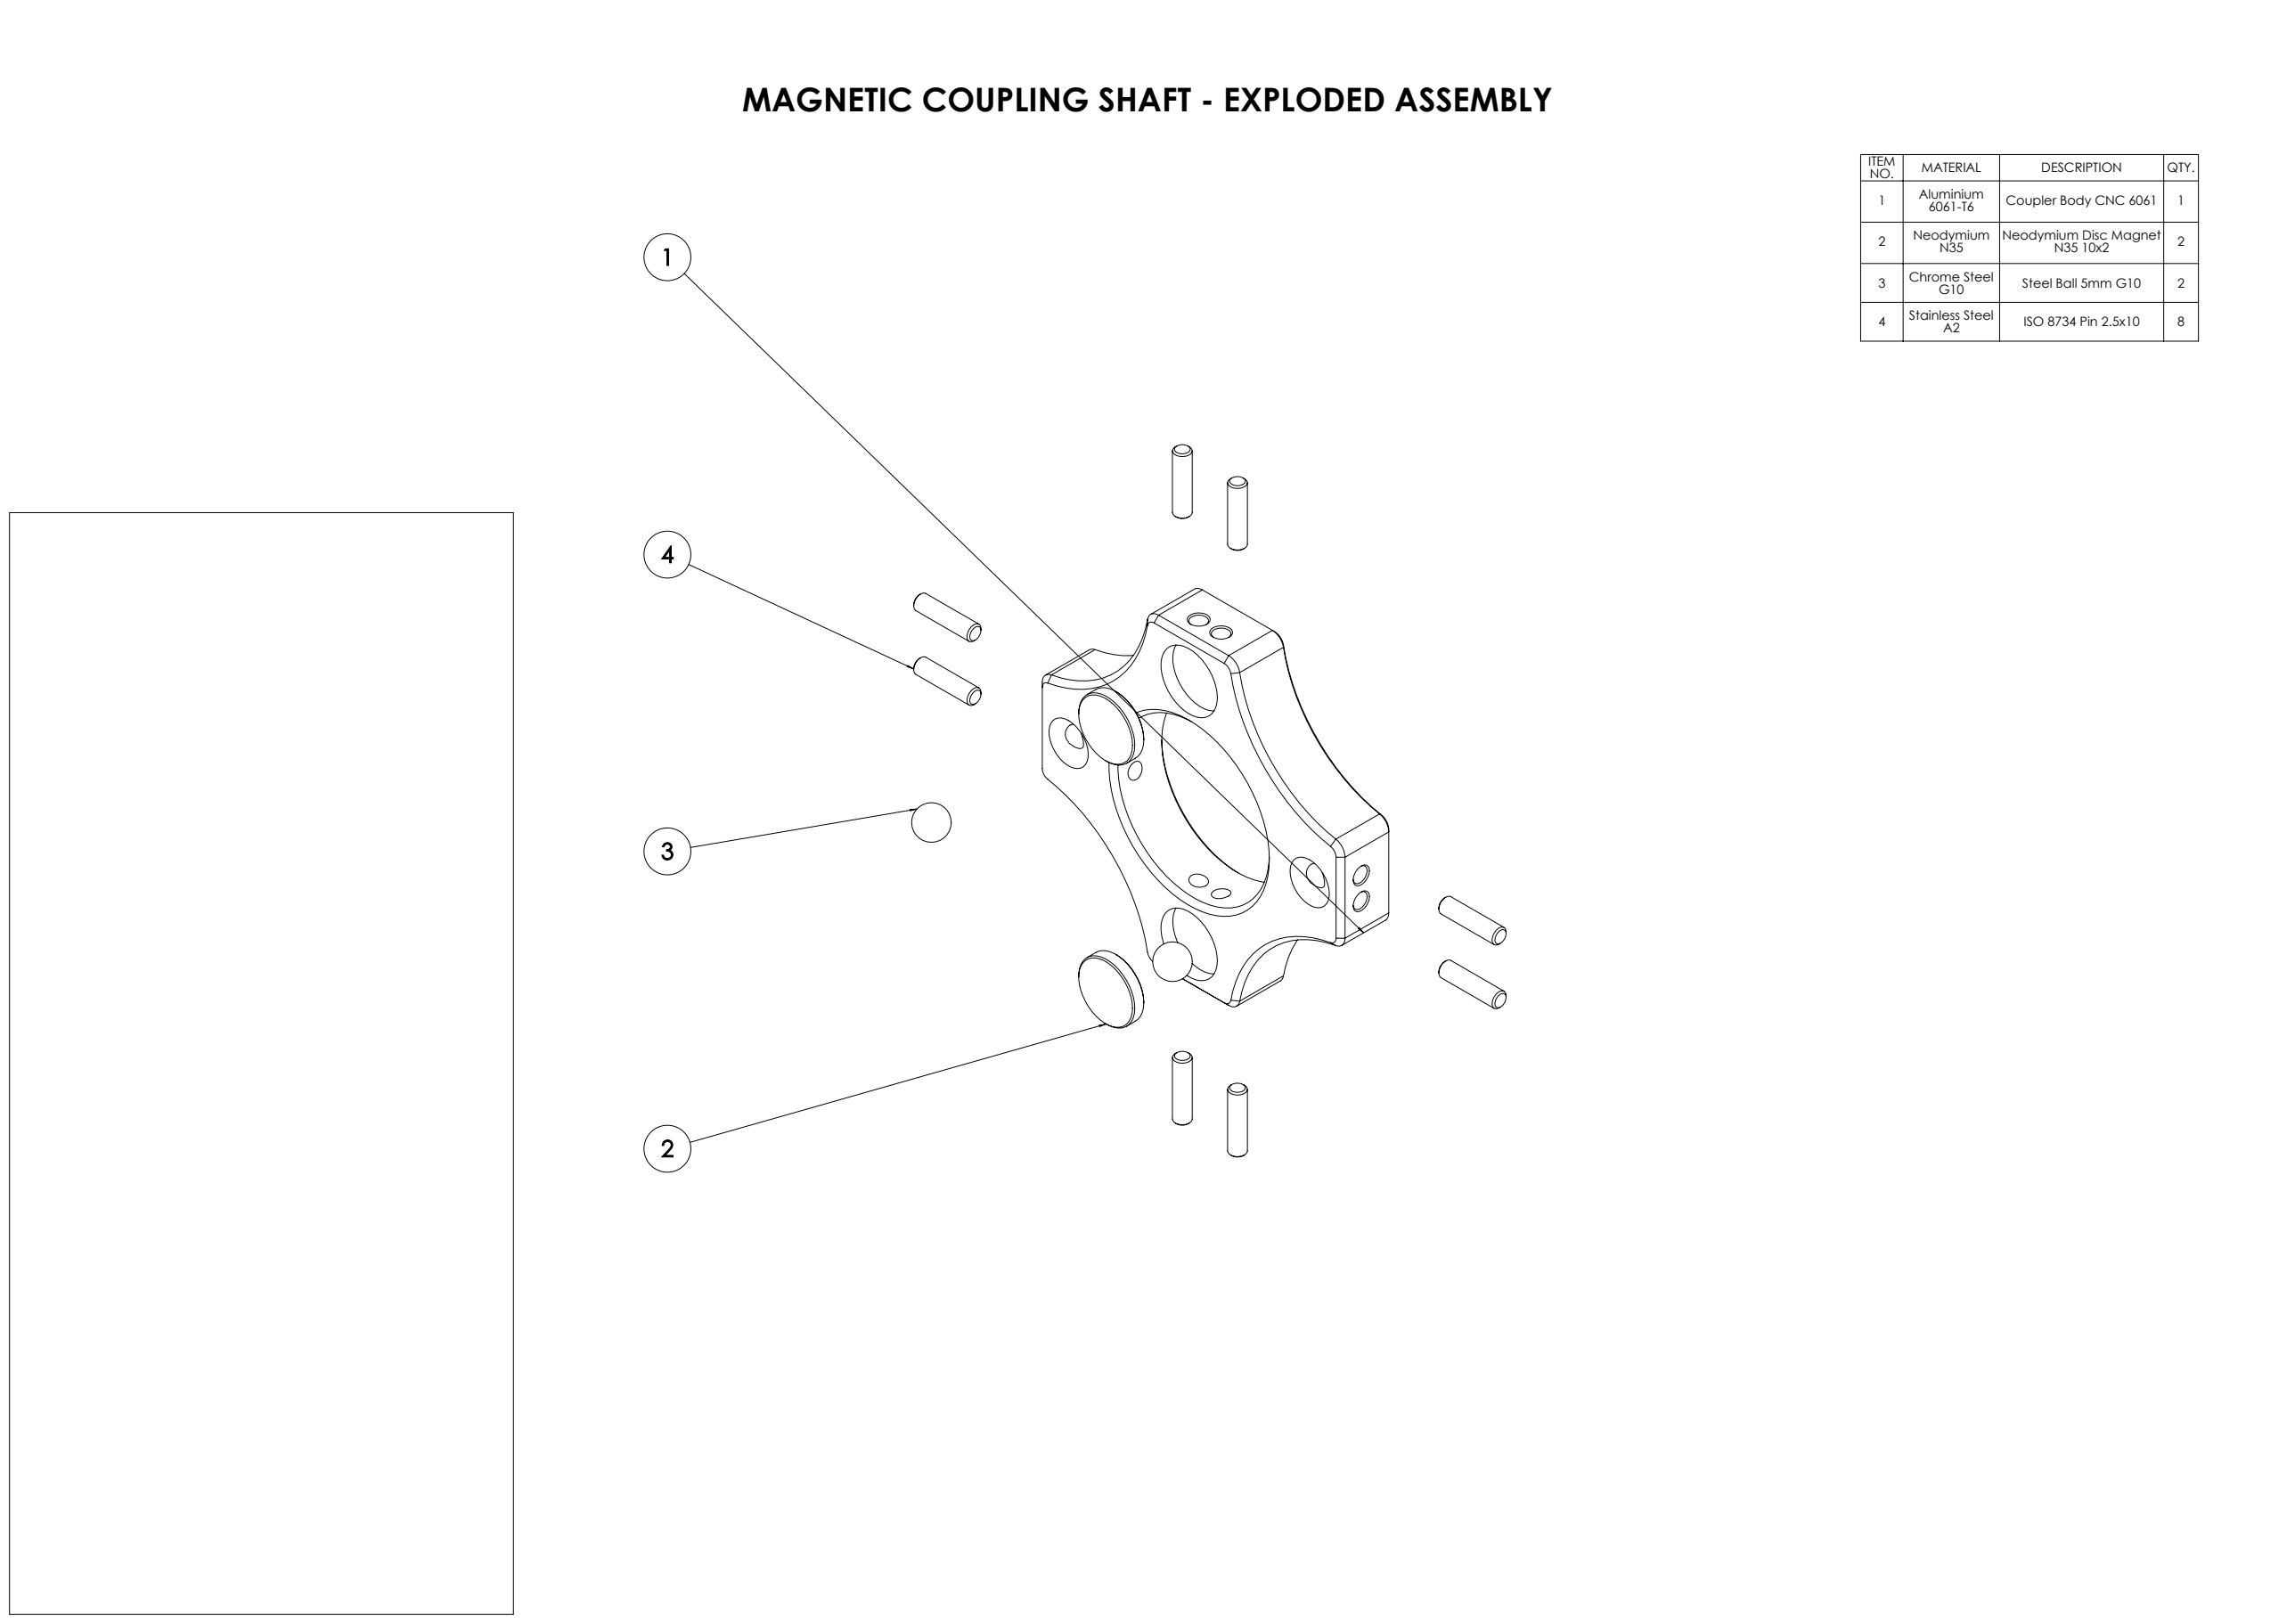
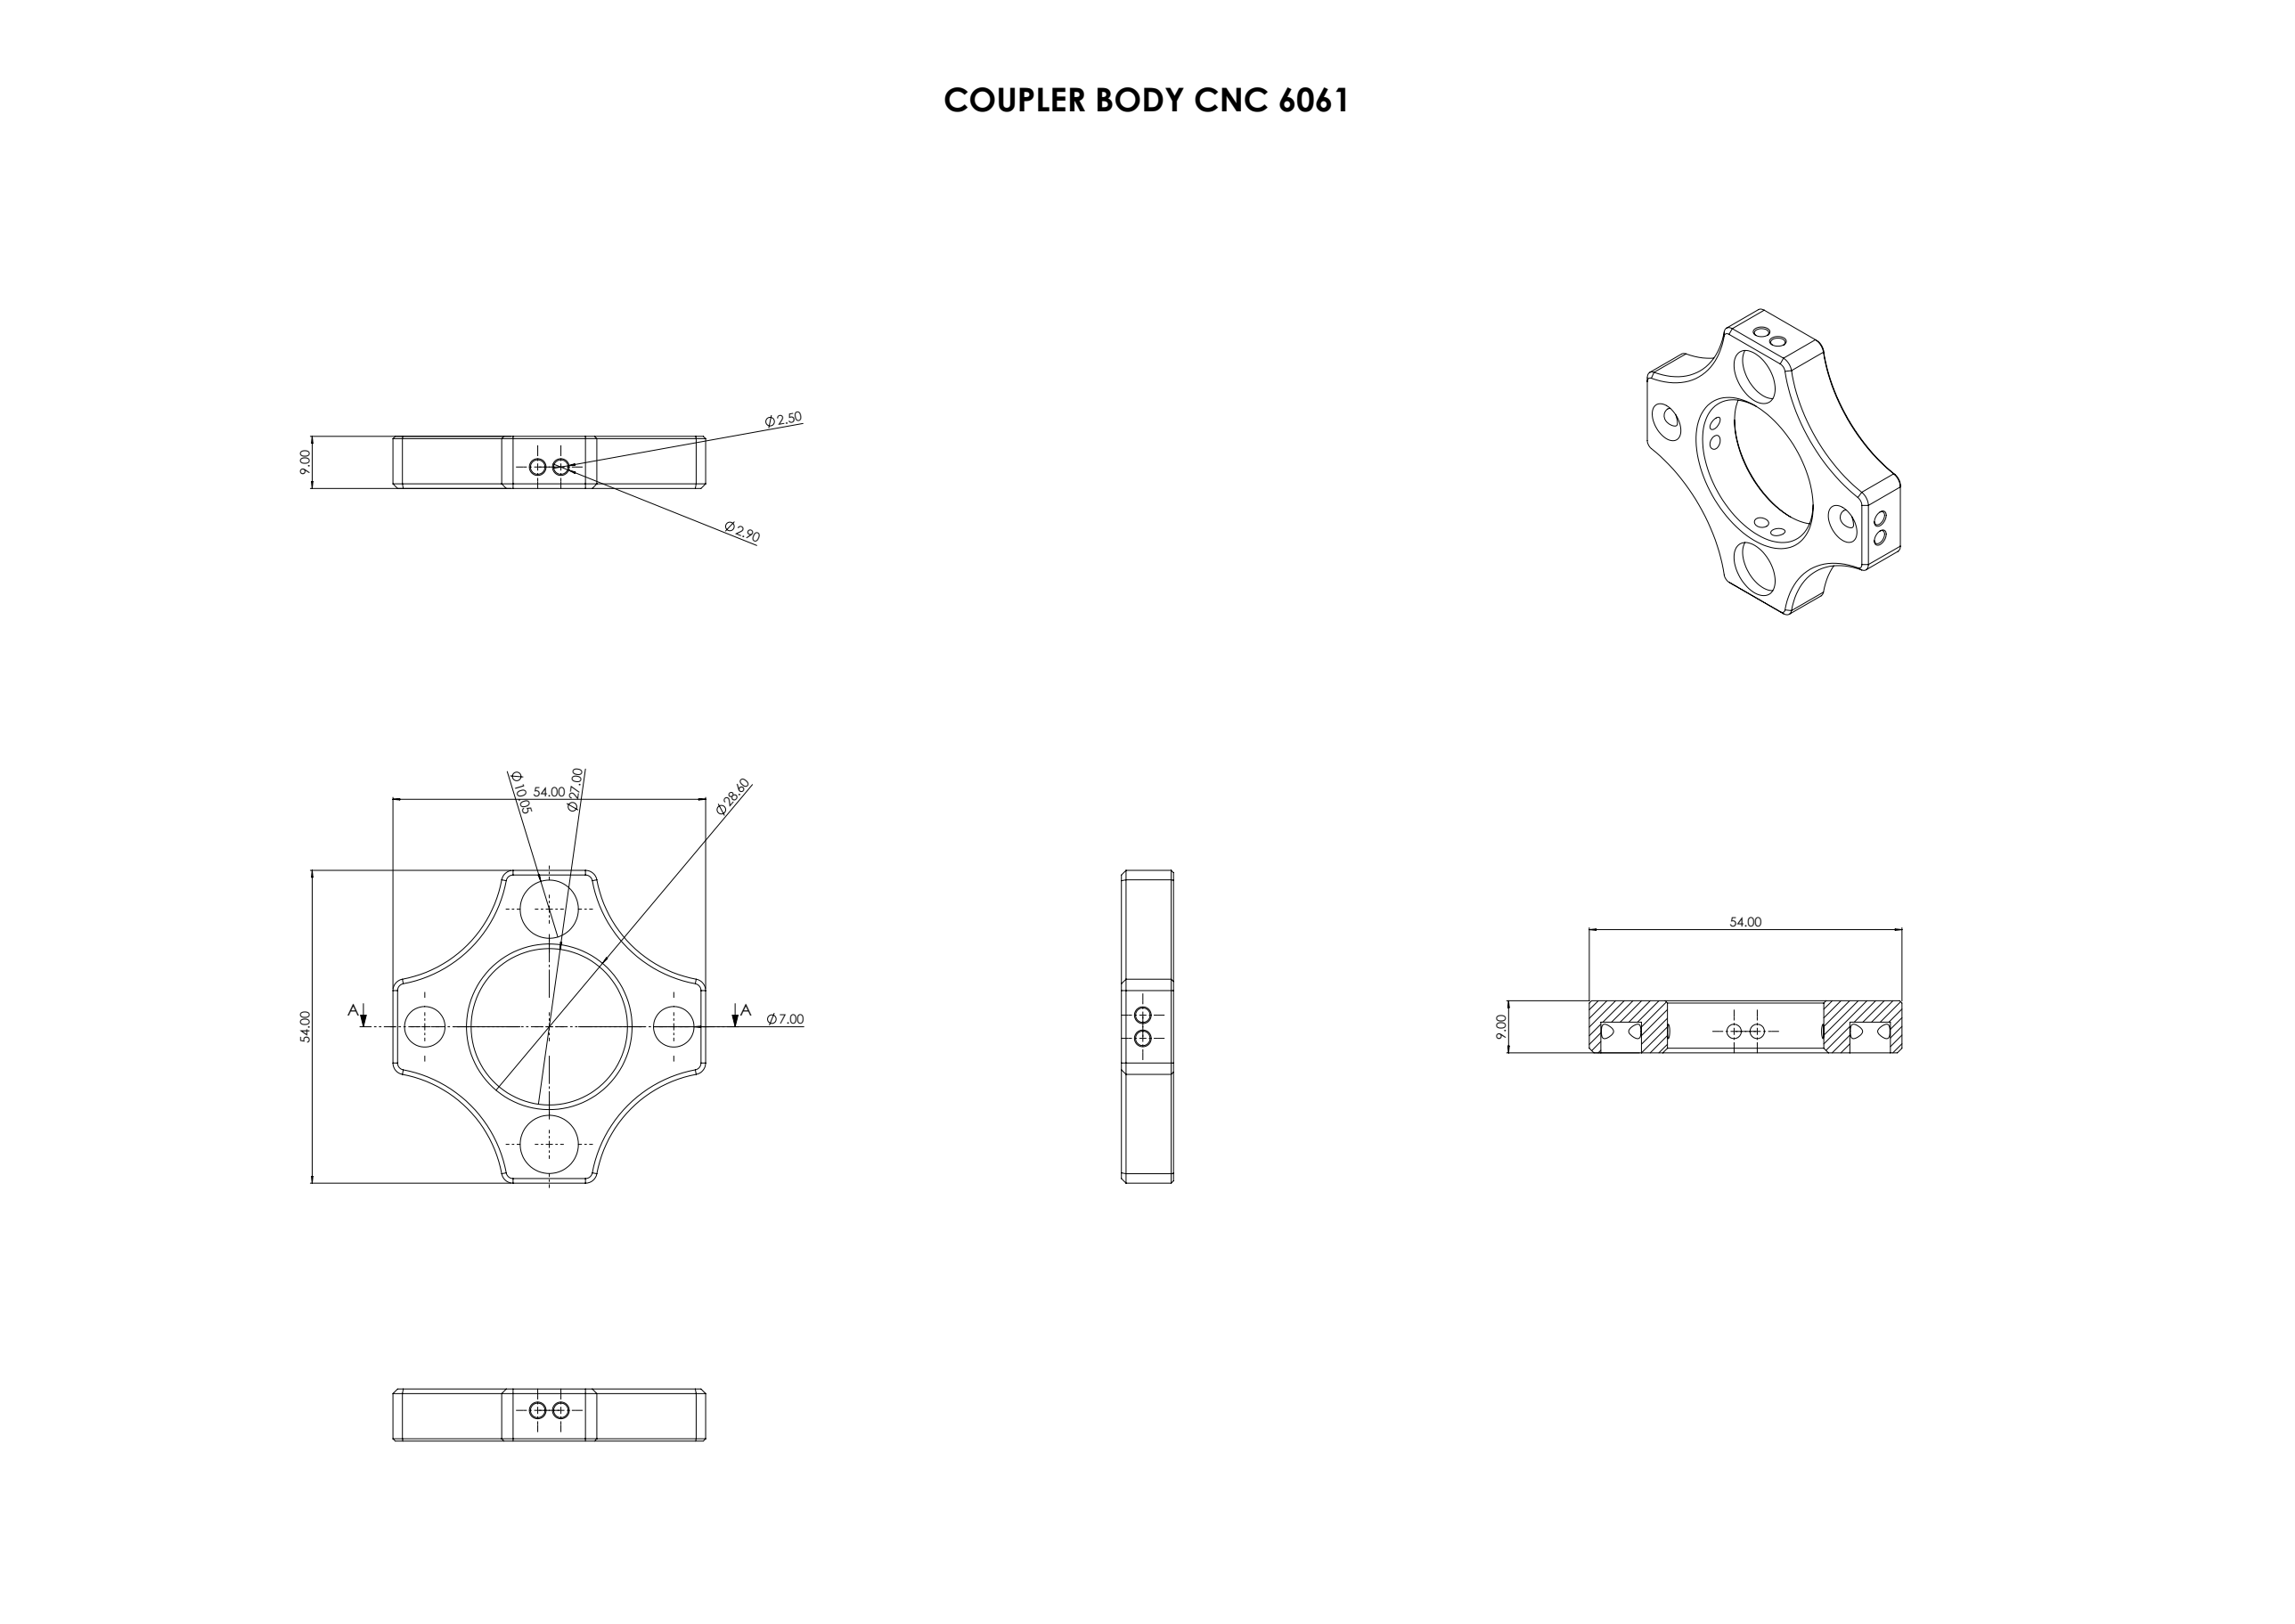
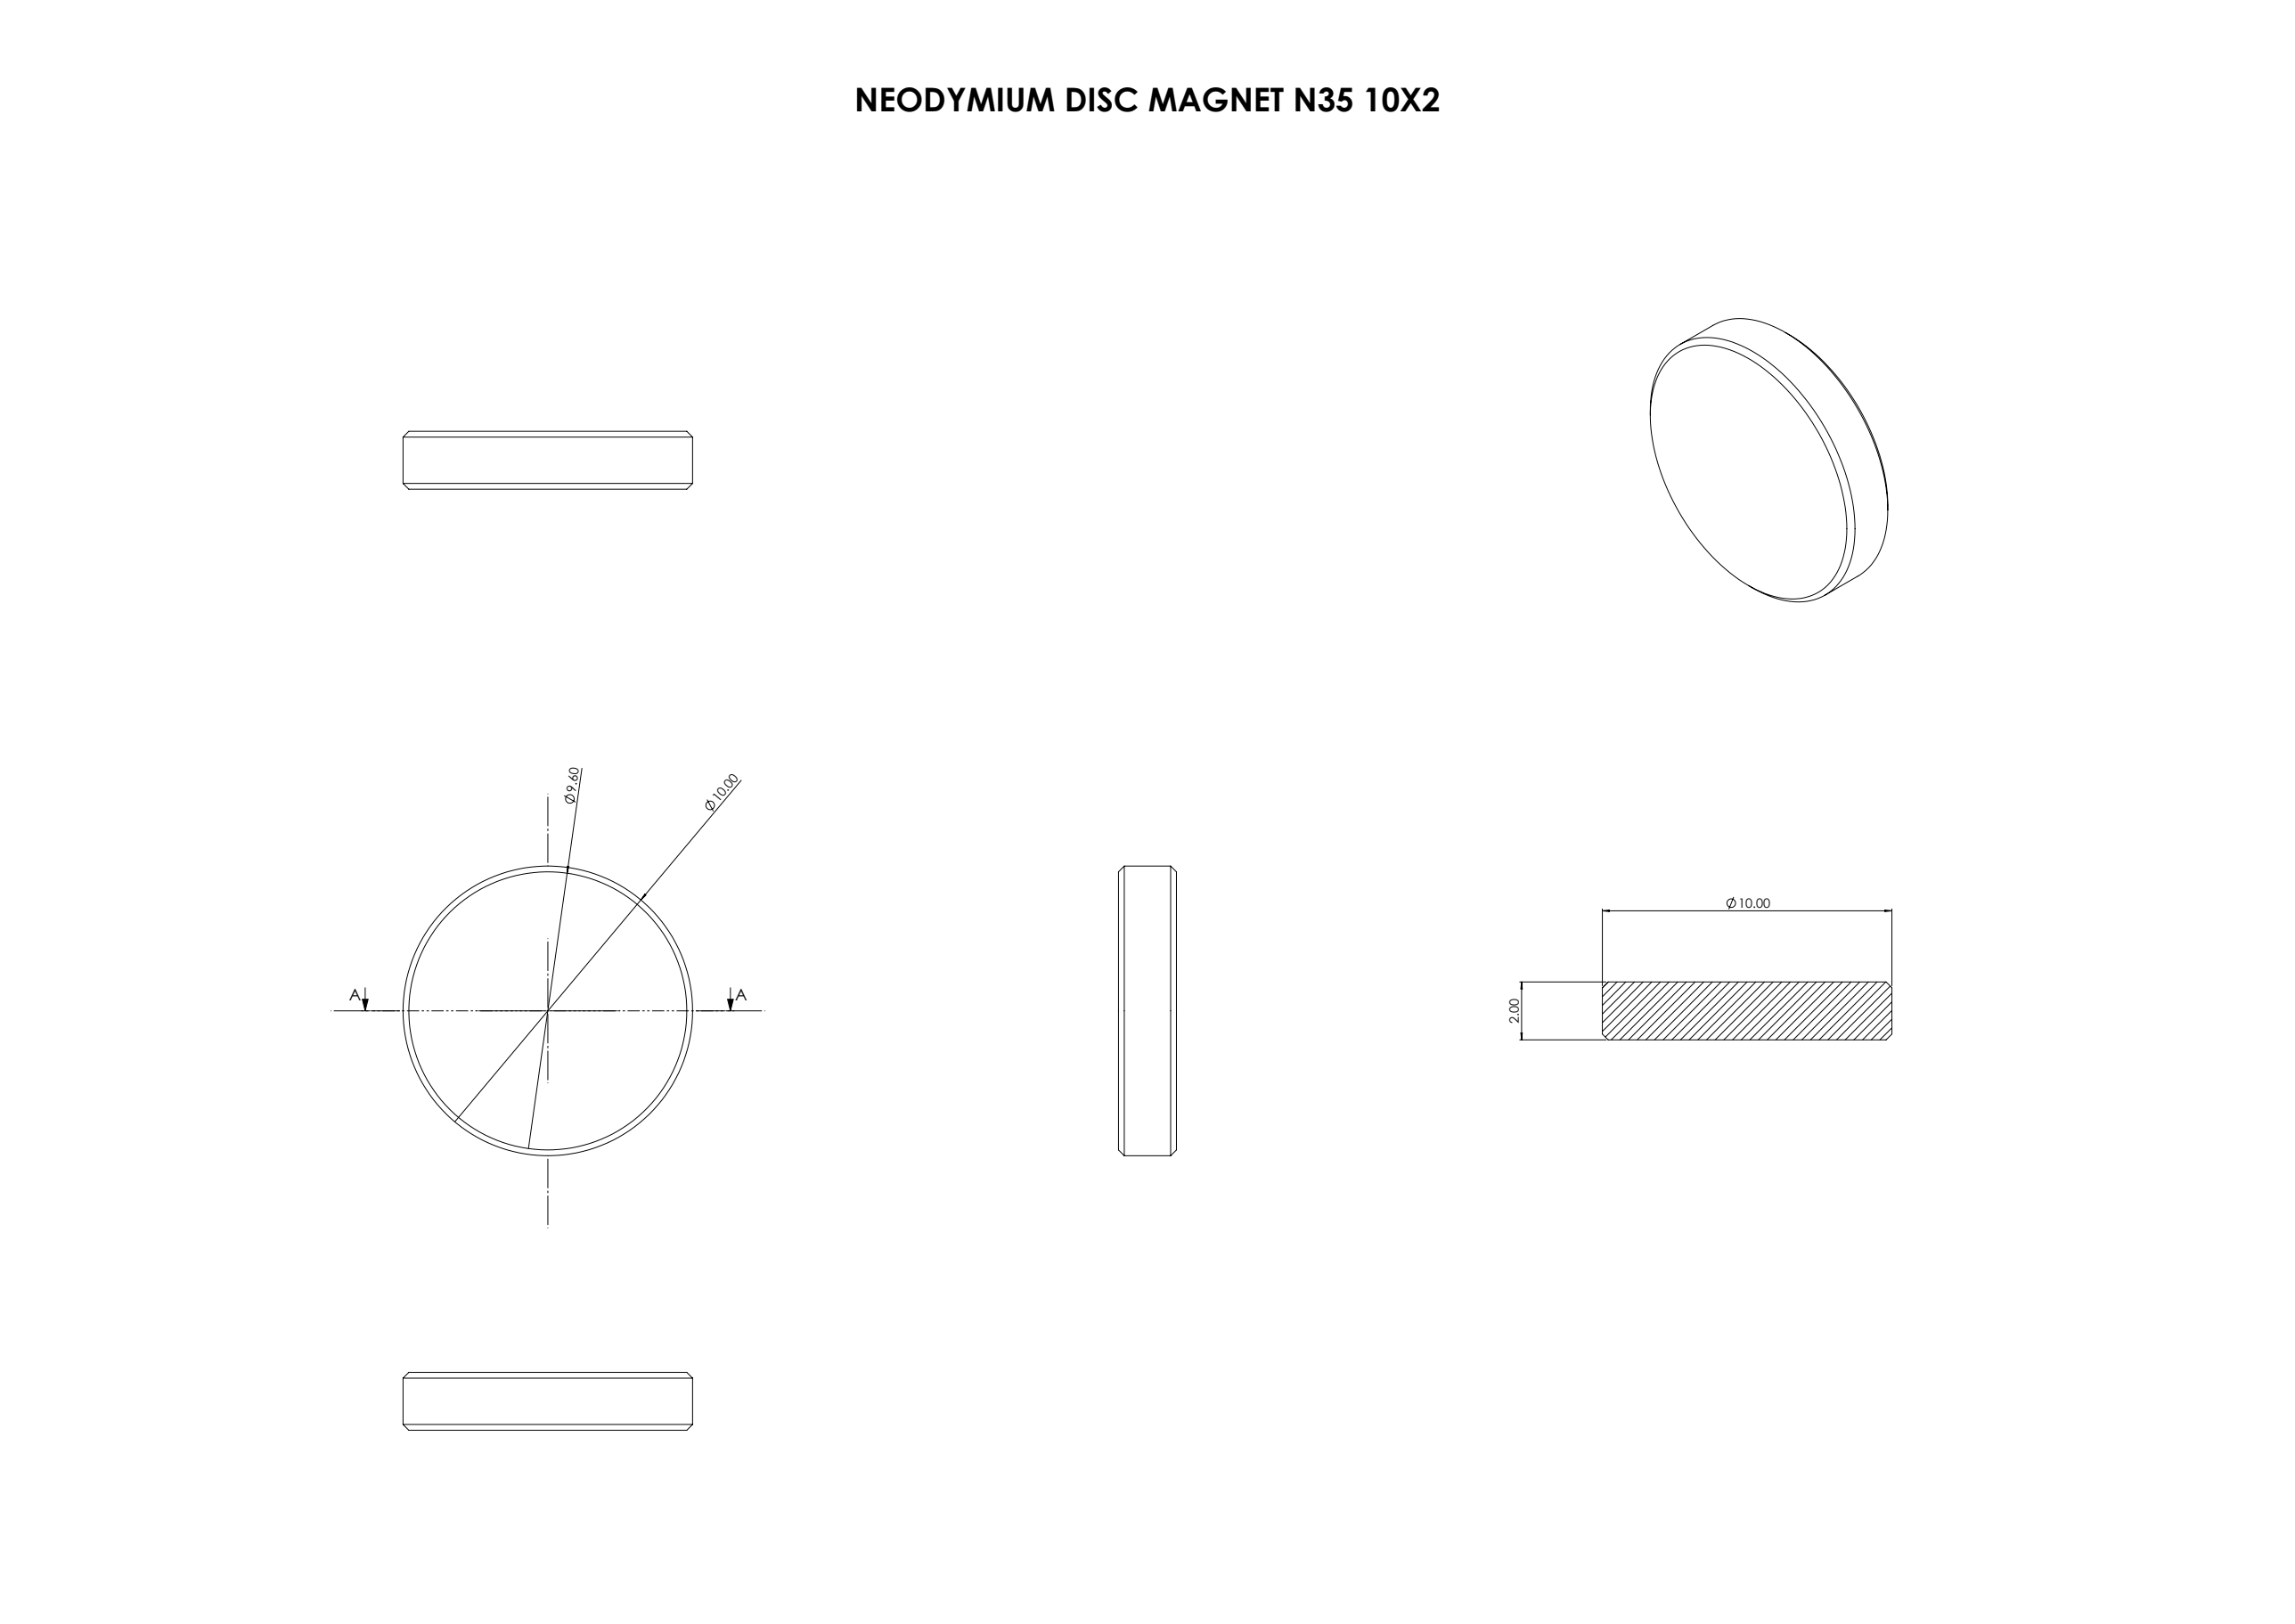
ISO-10303-21;
HEADER;
/* Generated by software containing ST-Developer
 * from STEP Tools, Inc. (www.steptools.com) 
 */

FILE_DESCRIPTION(
/* description */ (''),
/* implementation_level */ '2;1');

FILE_NAME(
/* name */ 'MAS-363',
/* time_stamp */ '2026-10-11T08:53:36-07:00',
/* author */ (''),
/* organization */ (''),
/* preprocessor_version */ 'ST-DEVELOPER v20.2',
/* originating_system */ 'Autodesk Translation Framework v15.15.0.0',
/* authorisation */ '');

FILE_SCHEMA (('AUTOMOTIVE_DESIGN { 1 0 10303 214 3 1 1 }'));
ENDSEC;

DATA;
#10=MECHANICAL_DESIGN_GEOMETRIC_PRESENTATION_REPRESENTATION('',(#72,#73,
#74,#75),#3338);
#11=ITEM_DEFINED_TRANSFORMATION($,$,#1624,#1805);
#12=ITEM_DEFINED_TRANSFORMATION($,$,#1782,#1806);
#13=ITEM_DEFINED_TRANSFORMATION($,$,#1782,#1807);
#14=ITEM_DEFINED_TRANSFORMATION($,$,#1792,#1808);
#15=ITEM_DEFINED_TRANSFORMATION($,$,#1792,#1809);
#16=ITEM_DEFINED_TRANSFORMATION($,$,#1795,#1810);
#17=ITEM_DEFINED_TRANSFORMATION($,$,#1795,#1811);
#18=ITEM_DEFINED_TRANSFORMATION($,$,#1795,#1812);
#19=ITEM_DEFINED_TRANSFORMATION($,$,#1795,#1813);
#20=ITEM_DEFINED_TRANSFORMATION($,$,#1795,#1814);
#21=ITEM_DEFINED_TRANSFORMATION($,$,#1795,#1815);
#22=ITEM_DEFINED_TRANSFORMATION($,$,#1795,#1816);
#23=ITEM_DEFINED_TRANSFORMATION($,$,#1795,#1817);
#24=(
REPRESENTATION_RELATIONSHIP($,$,#3367,#3366)
REPRESENTATION_RELATIONSHIP_WITH_TRANSFORMATION(#11)
SHAPE_REPRESENTATION_RELATIONSHIP()
);
#25=(
REPRESENTATION_RELATIONSHIP($,$,#3368,#3366)
REPRESENTATION_RELATIONSHIP_WITH_TRANSFORMATION(#12)
SHAPE_REPRESENTATION_RELATIONSHIP()
);
#26=(
REPRESENTATION_RELATIONSHIP($,$,#3368,#3366)
REPRESENTATION_RELATIONSHIP_WITH_TRANSFORMATION(#13)
SHAPE_REPRESENTATION_RELATIONSHIP()
);
#27=(
REPRESENTATION_RELATIONSHIP($,$,#3369,#3366)
REPRESENTATION_RELATIONSHIP_WITH_TRANSFORMATION(#14)
SHAPE_REPRESENTATION_RELATIONSHIP()
);
#28=(
REPRESENTATION_RELATIONSHIP($,$,#3369,#3366)
REPRESENTATION_RELATIONSHIP_WITH_TRANSFORMATION(#15)
SHAPE_REPRESENTATION_RELATIONSHIP()
);
#29=(
REPRESENTATION_RELATIONSHIP($,$,#3370,#3366)
REPRESENTATION_RELATIONSHIP_WITH_TRANSFORMATION(#16)
SHAPE_REPRESENTATION_RELATIONSHIP()
);
#30=(
REPRESENTATION_RELATIONSHIP($,$,#3370,#3366)
REPRESENTATION_RELATIONSHIP_WITH_TRANSFORMATION(#17)
SHAPE_REPRESENTATION_RELATIONSHIP()
);
#31=(
REPRESENTATION_RELATIONSHIP($,$,#3370,#3366)
REPRESENTATION_RELATIONSHIP_WITH_TRANSFORMATION(#18)
SHAPE_REPRESENTATION_RELATIONSHIP()
);
#32=(
REPRESENTATION_RELATIONSHIP($,$,#3370,#3366)
REPRESENTATION_RELATIONSHIP_WITH_TRANSFORMATION(#19)
SHAPE_REPRESENTATION_RELATIONSHIP()
);
#33=(
REPRESENTATION_RELATIONSHIP($,$,#3370,#3366)
REPRESENTATION_RELATIONSHIP_WITH_TRANSFORMATION(#20)
SHAPE_REPRESENTATION_RELATIONSHIP()
);
#34=(
REPRESENTATION_RELATIONSHIP($,$,#3370,#3366)
REPRESENTATION_RELATIONSHIP_WITH_TRANSFORMATION(#21)
SHAPE_REPRESENTATION_RELATIONSHIP()
);
#35=(
REPRESENTATION_RELATIONSHIP($,$,#3370,#3366)
REPRESENTATION_RELATIONSHIP_WITH_TRANSFORMATION(#22)
SHAPE_REPRESENTATION_RELATIONSHIP()
);
#36=(
REPRESENTATION_RELATIONSHIP($,$,#3370,#3366)
REPRESENTATION_RELATIONSHIP_WITH_TRANSFORMATION(#23)
SHAPE_REPRESENTATION_RELATIONSHIP()
);
#37=CONTEXT_DEPENDENT_SHAPE_REPRESENTATION(#24,#3353);
#38=CONTEXT_DEPENDENT_SHAPE_REPRESENTATION(#25,#3354);
#39=CONTEXT_DEPENDENT_SHAPE_REPRESENTATION(#26,#3355);
#40=CONTEXT_DEPENDENT_SHAPE_REPRESENTATION(#27,#3356);
#41=CONTEXT_DEPENDENT_SHAPE_REPRESENTATION(#28,#3357);
#42=CONTEXT_DEPENDENT_SHAPE_REPRESENTATION(#29,#3358);
#43=CONTEXT_DEPENDENT_SHAPE_REPRESENTATION(#30,#3359);
#44=CONTEXT_DEPENDENT_SHAPE_REPRESENTATION(#31,#3360);
#45=CONTEXT_DEPENDENT_SHAPE_REPRESENTATION(#32,#3361);
#46=CONTEXT_DEPENDENT_SHAPE_REPRESENTATION(#33,#3362);
#47=CONTEXT_DEPENDENT_SHAPE_REPRESENTATION(#34,#3363);
#48=CONTEXT_DEPENDENT_SHAPE_REPRESENTATION(#35,#3364);
#49=CONTEXT_DEPENDENT_SHAPE_REPRESENTATION(#36,#3365);
#50=NEXT_ASSEMBLY_USAGE_OCCURRENCE('01_Coupler_Body_CNC_6061:2',
'01_Coupler_Body_CNC_6061:2','01_Coupler_Body_CNC_6061:2',#3372,#3373,
'01_Coupler_Body_CNC_6061:2');
#51=NEXT_ASSEMBLY_USAGE_OCCURRENCE(
'02_Neodymium_Disc_Magnet_N35_10x2:2',
'02_Neodymium_Disc_Magnet_N35_10x2:2',
'02_Neodymium_Disc_Magnet_N35_10x2:2',#3372,#3374,
'02_Neodymium_Disc_Magnet_N35_10x2:2');
#52=NEXT_ASSEMBLY_USAGE_OCCURRENCE(
'02_Neodymium_Disc_Magnet_N35_10x2:3',
'02_Neodymium_Disc_Magnet_N35_10x2:3',
'02_Neodymium_Disc_Magnet_N35_10x2:3',#3372,#3374,
'02_Neodymium_Disc_Magnet_N35_10x2:3');
#53=NEXT_ASSEMBLY_USAGE_OCCURRENCE('03_Steel_Ball_5mm_G10:2',
'03_Steel_Ball_5mm_G10:2','03_Steel_Ball_5mm_G10:2',#3372,#3375,
'03_Steel_Ball_5mm_G10:2');
#54=NEXT_ASSEMBLY_USAGE_OCCURRENCE('03_Steel_Ball_5mm_G10:3',
'03_Steel_Ball_5mm_G10:3','03_Steel_Ball_5mm_G10:3',#3372,#3375,
'03_Steel_Ball_5mm_G10:3');
#55=NEXT_ASSEMBLY_USAGE_OCCURRENCE('04_ISO_8734_Pin_2.5x10:2',
'04_ISO_8734_Pin_2.5x10:2','04_ISO_8734_Pin_2.5x10:2',#3372,#3376,
'04_ISO_8734_Pin_2.5x10:2');
#56=NEXT_ASSEMBLY_USAGE_OCCURRENCE('04_ISO_8734_Pin_2.5x10:3',
'04_ISO_8734_Pin_2.5x10:3','04_ISO_8734_Pin_2.5x10:3',#3372,#3376,
'04_ISO_8734_Pin_2.5x10:3');
#57=NEXT_ASSEMBLY_USAGE_OCCURRENCE('04_ISO_8734_Pin_2.5x10:4',
'04_ISO_8734_Pin_2.5x10:4','04_ISO_8734_Pin_2.5x10:4',#3372,#3376,
'04_ISO_8734_Pin_2.5x10:4');
#58=NEXT_ASSEMBLY_USAGE_OCCURRENCE('04_ISO_8734_Pin_2.5x10:5',
'04_ISO_8734_Pin_2.5x10:5','04_ISO_8734_Pin_2.5x10:5',#3372,#3376,
'04_ISO_8734_Pin_2.5x10:5');
#59=NEXT_ASSEMBLY_USAGE_OCCURRENCE('04_ISO_8734_Pin_2.5x10:6',
'04_ISO_8734_Pin_2.5x10:6','04_ISO_8734_Pin_2.5x10:6',#3372,#3376,
'04_ISO_8734_Pin_2.5x10:6');
#60=NEXT_ASSEMBLY_USAGE_OCCURRENCE('04_ISO_8734_Pin_2.5x10:7',
'04_ISO_8734_Pin_2.5x10:7','04_ISO_8734_Pin_2.5x10:7',#3372,#3376,
'04_ISO_8734_Pin_2.5x10:7');
#61=NEXT_ASSEMBLY_USAGE_OCCURRENCE('04_ISO_8734_Pin_2.5x10:8',
'04_ISO_8734_Pin_2.5x10:8','04_ISO_8734_Pin_2.5x10:8',#3372,#3376,
'04_ISO_8734_Pin_2.5x10:8');
#62=NEXT_ASSEMBLY_USAGE_OCCURRENCE('04_ISO_8734_Pin_2.5x10:9',
'04_ISO_8734_Pin_2.5x10:9','04_ISO_8734_Pin_2.5x10:9',#3372,#3376,
'04_ISO_8734_Pin_2.5x10:9');
#63=SPHERICAL_SURFACE('',#1793,2.5);
#64=SHAPE_REPRESENTATION_RELATIONSHIP('SRR','None',#3367,#68);
#65=SHAPE_REPRESENTATION_RELATIONSHIP('SRR','None',#3368,#69);
#66=SHAPE_REPRESENTATION_RELATIONSHIP('SRR','None',#3369,#70);
#67=SHAPE_REPRESENTATION_RELATIONSHIP('SRR','None',#3370,#71);
#68=ADVANCED_BREP_SHAPE_REPRESENTATION('',(#76),#3334);
#69=ADVANCED_BREP_SHAPE_REPRESENTATION('',(#77),#3335);
#70=ADVANCED_BREP_SHAPE_REPRESENTATION('',(#78),#3336);
#71=ADVANCED_BREP_SHAPE_REPRESENTATION('',(#79),#3337);
#72=STYLED_ITEM('',(#3436),#76);
#73=STYLED_ITEM('',(#3450),#77);
#74=STYLED_ITEM('',(#3443),#78);
#75=STYLED_ITEM('',(#3457),#79);
#76=MANIFOLD_SOLID_BREP('Body1',#1574);
#77=MANIFOLD_SOLID_BREP('Body1',#1575);
#78=MANIFOLD_SOLID_BREP('Body1',#1576);
#79=MANIFOLD_SOLID_BREP('Body1',#1577);
#80=B_SPLINE_CURVE_WITH_KNOTS('',3,(#2327,#2328,#2329,#2330,#2331,#2332,
#2333,#2334,#2335,#2336),.UNSPECIFIED.,.F.,.F.,(4,2,2,2,4),(0.,0.0466731196164697,
0.0933462392329394,0.146281754847064,0.199217270461189),.UNSPECIFIED.);
#81=B_SPLINE_CURVE_WITH_KNOTS('',3,(#2337,#2338,#2339,#2340,#2341,#2342,
#2343,#2344,#2345,#2346,#2347,#2348,#2349,#2350,#2351,#2352,#2353,#2354,
#2355,#2356,#2357,#2358,#2359,#2360,#2361,#2362,#2363,#2364,#2365,#2366),
 .UNSPECIFIED.,.F.,.F.,(4,2,2,2,2,2,2,2,2,2,2,2,2,2,4),(0.199217270461189,
0.269430202694905,0.339643134928622,0.393818540201201,0.42090624283749,
0.44799394547378,0.475081648110069,0.502169350746359,0.556344756018938,
0.626557688252654,0.696770620486371,0.749706136100495,0.80264165171462,
0.84931477133109,0.895987890947559),.UNSPECIFIED.);
#82=B_SPLINE_CURVE_WITH_KNOTS('',3,(#2389,#2390,#2391,#2392,#2393,#2394,
#2395,#2396,#2397,#2398,#2399,#2400,#2401,#2402,#2403,#2404,#2405,#2406,
#2407,#2408,#2409,#2410,#2411,#2412,#2413,#2414,#2415,#2416,#2417,#2418),
 .UNSPECIFIED.,.F.,.F.,(4,2,2,2,2,2,2,2,2,2,2,2,2,2,4),(0.,0.0466731196164697,
0.0933462392329393,0.146281754847064,0.199217270461189,0.269430202694905,
0.339643134928622,0.393818540201201,0.42090624283749,0.44799394547378,0.475081648110069,
0.502169350746358,0.556344756018937,0.626557688252654,0.69677062048637),
 .UNSPECIFIED.);
#83=B_SPLINE_CURVE_WITH_KNOTS('',3,(#2419,#2420,#2421,#2422,#2423,#2424,
#2425,#2426,#2427,#2428),.UNSPECIFIED.,.F.,.F.,(4,2,2,2,4),(0.69677062048637,
0.749706136100495,0.80264165171462,0.84931477133109,0.895987890947559),
 .UNSPECIFIED.);
#84=B_SPLINE_CURVE_WITH_KNOTS('',3,(#2436,#2437,#2438,#2439,#2440,#2441,
#2442,#2443,#2444,#2445,#2446,#2447),.UNSPECIFIED.,.F.,.F.,(4,2,2,2,2,4),
(0.,0.0270877026362895,0.054175405272579,0.108350810545158,0.178563742778874,
0.248776675012591),.UNSPECIFIED.);
#85=B_SPLINE_CURVE_WITH_KNOTS('',3,(#2448,#2449,#2450,#2451,#2452,#2453,
#2454,#2455,#2456,#2457,#2458,#2459,#2460,#2461,#2462,#2463,#2464,#2465,
#2466,#2467,#2468,#2469,#2470,#2471,#2472,#2473,#2474,#2475),
 .UNSPECIFIED.,.F.,.F.,(4,2,2,2,2,2,2,2,2,2,2,2,2,4),(0.248776675012591,
0.301712190626716,0.35464770624084,0.40132082585731,0.44799394547378,0.494667065090249,
0.541340184706719,0.594275700320844,0.647211215934968,0.717424148168685,
0.787637080402401,0.84181248567498,0.86890018831127,0.895987890947559),
 .UNSPECIFIED.);
#86=B_SPLINE_CURVE_WITH_KNOTS('',3,(#2485,#2486,#2487,#2488,#2489,#2490,
#2491,#2492,#2493,#2494,#2495,#2496,#2497,#2498,#2499,#2500,#2501,#2502,
#2503,#2504,#2505,#2506,#2507,#2508,#2509,#2510,#2511,#2512),
 .UNSPECIFIED.,.F.,.F.,(4,2,2,2,2,2,2,2,2,2,2,2,2,4),(0.,0.0270877026362894,
0.0541754052725788,0.108350810545158,0.178563742778874,0.248776675012591,
0.301712190626716,0.35464770624084,0.40132082585731,0.44799394547378,0.494667065090249,
0.541340184706719,0.594275700320844,0.647211215934968),.UNSPECIFIED.);
#87=B_SPLINE_CURVE_WITH_KNOTS('',3,(#2513,#2514,#2515,#2516,#2517,#2518,
#2519,#2520,#2521,#2522,#2523,#2524),.UNSPECIFIED.,.F.,.F.,(4,2,2,2,2,4),
(0.647211215934968,0.717424148168685,0.787637080402402,0.84181248567498,
0.86890018831127,0.895987890947559),.UNSPECIFIED.);
#88=B_SPLINE_CURVE_WITH_KNOTS('',3,(#2544,#2545,#2546,#2547,#2548,#2549,
#2550,#2551,#2552,#2553,#2554,#2555,#2556,#2557,#2558,#2559,#2560,#2561,
#2562,#2563,#2564,#2565,#2566,#2567,#2568,#2569,#2570,#2571,#2572,#2573,
#2574,#2575,#2576,#2577),.UNSPECIFIED.,.T.,.F.,(4,2,2,2,2,2,2,2,2,2,2,2,
2,2,2,2,4),(0.,0.0471177022580085,0.094235404516017,0.142168460352567,0.190101516189116,
0.237513099195747,0.284924682202378,0.331987109916568,0.379049537630759,
0.426111965344949,0.473174393059139,0.52058597606577,0.567997559072401,
0.615930614908951,0.6638636707455,0.710981373003508,0.758099075261517),
 .UNSPECIFIED.);
#89=B_SPLINE_CURVE_WITH_KNOTS('',3,(#2599,#2600,#2601,#2602,#2603,#2604,
#2605,#2606,#2607,#2608,#2609,#2610,#2611,#2612,#2613,#2614,#2615,#2616,
#2617,#2618,#2619,#2620,#2621,#2622,#2623,#2624,#2625,#2626,#2627,#2628,
#2629,#2630,#2631,#2632),.UNSPECIFIED.,.T.,.F.,(4,2,2,2,2,2,2,2,2,2,2,2,
2,2,2,2,4),(0.,0.0471177022580085,0.094235404516017,0.142168460352567,0.190101516189116,
0.237513099195747,0.284924682202378,0.331987109916568,0.379049537630758,
0.426111965344949,0.473174393059139,0.52058597606577,0.567997559072401,
0.615930614908951,0.6638636707455,0.710981373003509,0.758099075261517),
 .UNSPECIFIED.);
#90=B_SPLINE_CURVE_WITH_KNOTS('',3,(#2639,#2640,#2641,#2642,#2643,#2644,
#2645,#2646,#2647,#2648,#2649,#2650,#2651,#2652,#2653,#2654,#2655,#2656,
#2657,#2658,#2659,#2660,#2661,#2662,#2663,#2664,#2665,#2666,#2667,#2668,
#2669,#2670,#2671,#2672),.UNSPECIFIED.,.T.,.F.,(4,2,2,2,2,2,2,2,2,2,2,2,
2,2,2,2,4),(0.,0.0470624277141901,0.0941248554283803,0.141536438435011,
0.188948021441642,0.236881077278192,0.284814133114742,0.33193183537275,
0.379049537630759,0.426167239888767,0.473284942146776,0.521217997983325,
0.569151053819875,0.616562636826506,0.663974219833137,0.711036647547327,
0.758099075261517),.UNSPECIFIED.);
#91=B_SPLINE_CURVE_WITH_KNOTS('',3,(#2681,#2682,#2683,#2684,#2685,#2686,
#2687,#2688,#2689,#2690,#2691,#2692,#2693,#2694,#2695,#2696,#2697,#2698,
#2699,#2700,#2701,#2702,#2703,#2704,#2705,#2706,#2707,#2708,#2709,#2710,
#2711,#2712,#2713,#2714),.UNSPECIFIED.,.T.,.F.,(4,2,2,2,2,2,2,2,2,2,2,2,
2,2,2,2,4),(0.,0.0470624277141901,0.0941248554283803,0.141536438435011,
0.188948021441642,0.236881077278192,0.284814133114742,0.33193183537275,
0.379049537630759,0.426167239888767,0.473284942146776,0.521217997983325,
0.569151053819875,0.616562636826506,0.663974219833137,0.711036647547327,
0.758099075261517),.UNSPECIFIED.);
#92=B_SPLINE_CURVE_WITH_KNOTS('',3,(#2718,#2719,#2720,#2721,#2722,#2723,
#2724,#2725,#2726,#2727,#2728,#2729),.UNSPECIFIED.,.F.,.F.,(4,2,2,2,2,4),
(0.,0.0270877026362894,0.0541754052725789,0.108350810545158,0.178563742778874,
0.248776675012591),.UNSPECIFIED.);
#93=B_SPLINE_CURVE_WITH_KNOTS('',3,(#2730,#2731,#2732,#2733,#2734,#2735,
#2736,#2737,#2738,#2739,#2740,#2741,#2742,#2743,#2744,#2745,#2746,#2747,
#2748,#2749,#2750,#2751,#2752,#2753,#2754,#2755,#2756,#2757),
 .UNSPECIFIED.,.F.,.F.,(4,2,2,2,2,2,2,2,2,2,2,2,2,4),(0.248776675012591,
0.301712190626716,0.35464770624084,0.40132082585731,0.44799394547378,0.494667065090249,
0.541340184706719,0.594275700320844,0.647211215934968,0.717424148168685,
0.787637080402401,0.84181248567498,0.86890018831127,0.895987890947559),
 .UNSPECIFIED.);
#94=B_SPLINE_CURVE_WITH_KNOTS('',3,(#2761,#2762,#2763,#2764,#2765,#2766,
#2767,#2768,#2769,#2770,#2771,#2772,#2773,#2774,#2775,#2776,#2777,#2778,
#2779,#2780,#2781,#2782,#2783,#2784,#2785,#2786),.UNSPECIFIED.,.F.,.F.,
(4,2,2,2,2,2,2,2,2,2,2,2,4),(0.,0.0471177022580085,0.094235404516017,0.142168460352567,
0.190101516189116,0.237513099195747,0.284924682202378,0.331987109916568,
0.379049537630759,0.426111965344949,0.473174393059139,0.52058597606577,
0.567997559072401),.UNSPECIFIED.);
#95=B_SPLINE_CURVE_WITH_KNOTS('',3,(#2787,#2788,#2789,#2790,#2791,#2792,
#2793,#2794,#2795,#2796),.UNSPECIFIED.,.F.,.F.,(4,2,2,2,4),(0.567997559072401,
0.615930614908951,0.6638636707455,0.710981373003509,0.758099075261517),
 .UNSPECIFIED.);
#96=B_SPLINE_CURVE_WITH_KNOTS('',3,(#2800,#2801,#2802,#2803,#2804,#2805,
#2806,#2807,#2808,#2809),.UNSPECIFIED.,.F.,.F.,(4,2,2,2,4),(0.,0.0471177022580085,
0.094235404516017,0.142168460352567,0.190101516189116),.UNSPECIFIED.);
#97=B_SPLINE_CURVE_WITH_KNOTS('',3,(#2810,#2811,#2812,#2813,#2814,#2815,
#2816,#2817,#2818,#2819,#2820,#2821,#2822,#2823,#2824,#2825,#2826,#2827,
#2828,#2829,#2830,#2831,#2832,#2833,#2834,#2835),.UNSPECIFIED.,.F.,.F.,
(4,2,2,2,2,2,2,2,2,2,2,2,4),(0.190101516189116,0.237513099195747,0.284924682202378,
0.331987109916568,0.379049537630759,0.426111965344949,0.473174393059139,
0.52058597606577,0.567997559072401,0.615930614908951,0.6638636707455,0.710981373003509,
0.758099075261517),.UNSPECIFIED.);
#98=B_SPLINE_CURVE_WITH_KNOTS('',3,(#2839,#2840,#2841,#2842,#2843,#2844,
#2845,#2846,#2847,#2848,#2849,#2850,#2851,#2852,#2853,#2854,#2855,#2856,
#2857,#2858,#2859,#2860,#2861,#2862,#2863,#2864,#2865,#2866),
 .UNSPECIFIED.,.F.,.F.,(4,2,2,2,2,2,2,2,2,2,2,2,2,4),(0.,0.0270877026362895,
0.0541754052725789,0.108350810545158,0.178563742778874,0.248776675012591,
0.301712190626716,0.35464770624084,0.40132082585731,0.44799394547378,0.494667065090249,
0.541340184706719,0.594275700320844,0.647211215934968),.UNSPECIFIED.);
#99=B_SPLINE_CURVE_WITH_KNOTS('',3,(#2867,#2868,#2869,#2870,#2871,#2872,
#2873,#2874,#2875,#2876,#2877,#2878),.UNSPECIFIED.,.F.,.F.,(4,2,2,2,2,4),
(0.647211215934968,0.717424148168685,0.787637080402401,0.84181248567498,
0.86890018831127,0.895987890947559),.UNSPECIFIED.);
#100=B_SPLINE_CURVE_WITH_KNOTS('',3,(#2882,#2883,#2884,#2885,#2886,#2887,
#2888,#2889,#2890,#2891),.UNSPECIFIED.,.F.,.F.,(4,2,2,2,4),(0.,0.0466731196164697,
0.0933462392329394,0.146281754847064,0.199217270461189),.UNSPECIFIED.);
#101=B_SPLINE_CURVE_WITH_KNOTS('',3,(#2892,#2893,#2894,#2895,#2896,#2897,
#2898,#2899,#2900,#2901,#2902,#2903,#2904,#2905,#2906,#2907,#2908,#2909,
#2910,#2911,#2912,#2913,#2914,#2915,#2916,#2917,#2918,#2919,#2920,#2921),
 .UNSPECIFIED.,.F.,.F.,(4,2,2,2,2,2,2,2,2,2,2,2,2,2,4),(0.199217270461189,
0.269430202694905,0.339643134928622,0.393818540201201,0.42090624283749,
0.44799394547378,0.475081648110069,0.502169350746359,0.556344756018938,
0.626557688252654,0.696770620486371,0.749706136100496,0.80264165171462,
0.84931477133109,0.89598789094756),.UNSPECIFIED.);
#102=B_SPLINE_CURVE_WITH_KNOTS('',3,(#2925,#2926,#2927,#2928,#2929,#2930,
#2931,#2932,#2933,#2934,#2935,#2936,#2937,#2938,#2939,#2940,#2941,#2942,
#2943,#2944,#2945,#2946,#2947,#2948,#2949,#2950),.UNSPECIFIED.,.F.,.F.,
(4,2,2,2,2,2,2,2,2,2,2,2,4),(0.,0.0470624277141902,0.0941248554283803,0.141536438435011,
0.188948021441642,0.236881077278192,0.284814133114742,0.33193183537275,
0.379049537630759,0.426167239888767,0.473284942146776,0.521217997983325,
0.569151053819875),.UNSPECIFIED.);
#103=B_SPLINE_CURVE_WITH_KNOTS('',3,(#2951,#2952,#2953,#2954,#2955,#2956,
#2957,#2958,#2959,#2960),.UNSPECIFIED.,.F.,.F.,(4,2,2,2,4),(0.569151053819875,
0.616562636826506,0.663974219833137,0.711036647547327,0.758099075261517),
 .UNSPECIFIED.);
#104=B_SPLINE_CURVE_WITH_KNOTS('',3,(#2964,#2965,#2966,#2967,#2968,#2969,
#2970,#2971,#2972,#2973),.UNSPECIFIED.,.F.,.F.,(4,2,2,2,4),(0.,0.0470624277141902,
0.0941248554283803,0.141536438435011,0.188948021441642),.UNSPECIFIED.);
#105=B_SPLINE_CURVE_WITH_KNOTS('',3,(#2974,#2975,#2976,#2977,#2978,#2979,
#2980,#2981,#2982,#2983,#2984,#2985,#2986,#2987,#2988,#2989,#2990,#2991,
#2992,#2993,#2994,#2995,#2996,#2997,#2998,#2999),.UNSPECIFIED.,.F.,.F.,
(4,2,2,2,2,2,2,2,2,2,2,2,4),(0.188948021441642,0.236881077278192,0.284814133114742,
0.33193183537275,0.379049537630759,0.426167239888767,0.473284942146776,
0.521217997983325,0.569151053819875,0.616562636826506,0.663974219833137,
0.711036647547327,0.758099075261517),.UNSPECIFIED.);
#106=B_SPLINE_CURVE_WITH_KNOTS('',3,(#3003,#3004,#3005,#3006,#3007,#3008,
#3009,#3010,#3011,#3012,#3013,#3014,#3015,#3016,#3017,#3018,#3019,#3020,
#3021,#3022,#3023,#3024,#3025,#3026,#3027,#3028,#3029,#3030,#3031,#3032),
 .UNSPECIFIED.,.F.,.F.,(4,2,2,2,2,2,2,2,2,2,2,2,2,2,4),(0.,0.0466731196164697,
0.0933462392329393,0.146281754847064,0.199217270461189,0.269430202694905,
0.339643134928622,0.393818540201201,0.42090624283749,0.44799394547378,0.475081648110069,
0.502169350746358,0.556344756018937,0.626557688252654,0.69677062048637),
 .UNSPECIFIED.);
#107=B_SPLINE_CURVE_WITH_KNOTS('',3,(#3033,#3034,#3035,#3036,#3037,#3038,
#3039,#3040,#3041,#3042),.UNSPECIFIED.,.F.,.F.,(4,2,2,2,4),(0.69677062048637,
0.749706136100495,0.80264165171462,0.849314771331089,0.895987890947559),
 .UNSPECIFIED.);
#108=CYLINDRICAL_SURFACE('',#1630,1.25);
#109=CYLINDRICAL_SURFACE('',#1636,1.25);
#110=CYLINDRICAL_SURFACE('',#1639,1.25);
#111=CYLINDRICAL_SURFACE('',#1642,1.25);
#112=CYLINDRICAL_SURFACE('',#1648,1.25);
#113=CYLINDRICAL_SURFACE('',#1654,1.25);
#114=CYLINDRICAL_SURFACE('',#1657,1.25);
#115=CYLINDRICAL_SURFACE('',#1660,1.25);
#116=CYLINDRICAL_SURFACE('',#1661,1.25);
#117=CYLINDRICAL_SURFACE('',#1662,1.25);
#118=CYLINDRICAL_SURFACE('',#1663,1.25);
#119=CYLINDRICAL_SURFACE('',#1664,1.25);
#120=CYLINDRICAL_SURFACE('',#1665,3.5);
#121=CYLINDRICAL_SURFACE('',#1669,3.5);
#122=CYLINDRICAL_SURFACE('',#1673,5.025);
#123=CYLINDRICAL_SURFACE('',#1677,5.025);
#124=CYLINDRICAL_SURFACE('',#1721,2.);
#125=CYLINDRICAL_SURFACE('',#1723,21.4);
#126=CYLINDRICAL_SURFACE('',#1725,2.);
#127=CYLINDRICAL_SURFACE('',#1727,2.);
#128=CYLINDRICAL_SURFACE('',#1729,21.4);
#129=CYLINDRICAL_SURFACE('',#1731,2.);
#130=CYLINDRICAL_SURFACE('',#1737,13.5);
#131=CYLINDRICAL_SURFACE('',#1776,2.);
#132=CYLINDRICAL_SURFACE('',#1777,2.);
#133=CYLINDRICAL_SURFACE('',#1778,2.);
#134=CYLINDRICAL_SURFACE('',#1779,2.);
#135=CYLINDRICAL_SURFACE('',#1780,21.4);
#136=CYLINDRICAL_SURFACE('',#1781,21.4);
#137=CYLINDRICAL_SURFACE('',#1786,5.);
#138=CYLINDRICAL_SURFACE('',#1800,1.25);
#139=FACE_BOUND('',#285,.T.);
#140=FACE_BOUND('',#286,.T.);
#141=FACE_BOUND('',#290,.T.);
#142=FACE_BOUND('',#291,.T.);
#143=FACE_BOUND('',#299,.T.);
#144=FACE_BOUND('',#300,.T.);
#145=FACE_BOUND('',#304,.T.);
#146=FACE_BOUND('',#305,.T.);
#147=FACE_BOUND('',#316,.T.);
#148=FACE_BOUND('',#317,.T.);
#149=FACE_BOUND('',#318,.T.);
#150=FACE_BOUND('',#319,.T.);
#151=FACE_BOUND('',#322,.T.);
#152=FACE_BOUND('',#323,.T.);
#153=FACE_BOUND('',#324,.T.);
#154=FACE_BOUND('',#325,.T.);
#155=FACE_BOUND('',#354,.T.);
#156=FACE_BOUND('',#357,.T.);
#157=FACE_BOUND('',#358,.T.);
#158=FACE_BOUND('',#359,.T.);
#159=FACE_BOUND('',#360,.T.);
#160=FACE_BOUND('',#361,.T.);
#161=FACE_BOUND('',#362,.T.);
#162=FACE_BOUND('',#363,.T.);
#163=FACE_BOUND('',#364,.T.);
#164=FACE_BOUND('',#367,.T.);
#165=FACE_BOUND('',#368,.T.);
#166=FACE_BOUND('',#369,.T.);
#167=FACE_BOUND('',#370,.T.);
#168=FACE_BOUND('',#371,.T.);
#169=PLANE('',#1628);
#170=PLANE('',#1634);
#171=PLANE('',#1646);
#172=PLANE('',#1652);
#173=PLANE('',#1668);
#174=PLANE('',#1672);
#175=PLANE('',#1676);
#176=PLANE('',#1680);
#177=PLANE('',#1681);
#178=PLANE('',#1691);
#179=PLANE('',#1701);
#180=PLANE('',#1711);
#181=PLANE('',#1733);
#182=PLANE('',#1741);
#183=PLANE('',#1755);
#184=PLANE('',#1762);
#185=PLANE('',#1769);
#186=PLANE('',#1773);
#187=PLANE('',#1788);
#188=PLANE('',#1791);
#189=PLANE('',#1796);
#190=PLANE('',#1804);
#191=FACE_OUTER_BOUND('',#283,.T.);
#192=FACE_OUTER_BOUND('',#284,.T.);
#193=FACE_OUTER_BOUND('',#287,.T.);
#194=FACE_OUTER_BOUND('',#288,.T.);
#195=FACE_OUTER_BOUND('',#289,.T.);
#196=FACE_OUTER_BOUND('',#292,.T.);
#197=FACE_OUTER_BOUND('',#293,.T.);
#198=FACE_OUTER_BOUND('',#294,.T.);
#199=FACE_OUTER_BOUND('',#295,.T.);
#200=FACE_OUTER_BOUND('',#296,.T.);
#201=FACE_OUTER_BOUND('',#297,.T.);
#202=FACE_OUTER_BOUND('',#298,.T.);
#203=FACE_OUTER_BOUND('',#301,.T.);
#204=FACE_OUTER_BOUND('',#302,.T.);
#205=FACE_OUTER_BOUND('',#303,.T.);
#206=FACE_OUTER_BOUND('',#306,.T.);
#207=FACE_OUTER_BOUND('',#307,.T.);
#208=FACE_OUTER_BOUND('',#308,.T.);
#209=FACE_OUTER_BOUND('',#309,.T.);
#210=FACE_OUTER_BOUND('',#310,.T.);
#211=FACE_OUTER_BOUND('',#311,.T.);
#212=FACE_OUTER_BOUND('',#312,.T.);
#213=FACE_OUTER_BOUND('',#313,.T.);
#214=FACE_OUTER_BOUND('',#314,.T.);
#215=FACE_OUTER_BOUND('',#315,.T.);
#216=FACE_OUTER_BOUND('',#320,.T.);
#217=FACE_OUTER_BOUND('',#321,.T.);
#218=FACE_OUTER_BOUND('',#326,.T.);
#219=FACE_OUTER_BOUND('',#327,.T.);
#220=FACE_OUTER_BOUND('',#328,.T.);
#221=FACE_OUTER_BOUND('',#329,.T.);
#222=FACE_OUTER_BOUND('',#330,.T.);
#223=FACE_OUTER_BOUND('',#331,.T.);
#224=FACE_OUTER_BOUND('',#332,.T.);
#225=FACE_OUTER_BOUND('',#333,.T.);
#226=FACE_OUTER_BOUND('',#334,.T.);
#227=FACE_OUTER_BOUND('',#335,.T.);
#228=FACE_OUTER_BOUND('',#336,.T.);
#229=FACE_OUTER_BOUND('',#337,.T.);
#230=FACE_OUTER_BOUND('',#338,.T.);
#231=FACE_OUTER_BOUND('',#339,.T.);
#232=FACE_OUTER_BOUND('',#340,.T.);
#233=FACE_OUTER_BOUND('',#341,.T.);
#234=FACE_OUTER_BOUND('',#342,.T.);
#235=FACE_OUTER_BOUND('',#343,.T.);
#236=FACE_OUTER_BOUND('',#344,.T.);
#237=FACE_OUTER_BOUND('',#345,.T.);
#238=FACE_OUTER_BOUND('',#346,.T.);
#239=FACE_OUTER_BOUND('',#347,.T.);
#240=FACE_OUTER_BOUND('',#348,.T.);
#241=FACE_OUTER_BOUND('',#349,.T.);
#242=FACE_OUTER_BOUND('',#350,.T.);
#243=FACE_OUTER_BOUND('',#351,.T.);
#244=FACE_OUTER_BOUND('',#352,.T.);
#245=FACE_OUTER_BOUND('',#353,.T.);
#246=FACE_OUTER_BOUND('',#355,.T.);
#247=FACE_OUTER_BOUND('',#356,.T.);
#248=FACE_OUTER_BOUND('',#365,.T.);
#249=FACE_OUTER_BOUND('',#366,.T.);
#250=FACE_OUTER_BOUND('',#372,.T.);
#251=FACE_OUTER_BOUND('',#373,.T.);
#252=FACE_OUTER_BOUND('',#374,.T.);
#253=FACE_OUTER_BOUND('',#375,.T.);
#254=FACE_OUTER_BOUND('',#376,.T.);
#255=FACE_OUTER_BOUND('',#377,.T.);
#256=FACE_OUTER_BOUND('',#378,.T.);
#257=FACE_OUTER_BOUND('',#379,.T.);
#258=FACE_OUTER_BOUND('',#380,.T.);
#259=FACE_OUTER_BOUND('',#381,.T.);
#260=FACE_OUTER_BOUND('',#382,.T.);
#261=FACE_OUTER_BOUND('',#383,.T.);
#262=FACE_OUTER_BOUND('',#384,.T.);
#263=FACE_OUTER_BOUND('',#385,.T.);
#264=FACE_OUTER_BOUND('',#386,.T.);
#265=FACE_OUTER_BOUND('',#387,.T.);
#266=FACE_OUTER_BOUND('',#388,.T.);
#267=FACE_OUTER_BOUND('',#389,.T.);
#268=FACE_OUTER_BOUND('',#390,.T.);
#269=FACE_OUTER_BOUND('',#391,.T.);
#270=FACE_OUTER_BOUND('',#392,.T.);
#271=FACE_OUTER_BOUND('',#393,.T.);
#272=FACE_OUTER_BOUND('',#394,.T.);
#273=FACE_OUTER_BOUND('',#395,.T.);
#274=FACE_OUTER_BOUND('',#396,.T.);
#275=FACE_OUTER_BOUND('',#397,.T.);
#276=FACE_OUTER_BOUND('',#398,.T.);
#277=FACE_OUTER_BOUND('',#399,.T.);
#278=FACE_OUTER_BOUND('',#400,.T.);
#279=FACE_OUTER_BOUND('',#401,.T.);
#280=FACE_OUTER_BOUND('',#402,.T.);
#281=FACE_OUTER_BOUND('',#403,.T.);
#282=FACE_OUTER_BOUND('',#404,.T.);
#283=EDGE_LOOP('',(#1024,#1025,#1026,#1027));
#284=EDGE_LOOP('',(#1028,#1029,#1030,#1031));
#285=EDGE_LOOP('',(#1032));
#286=EDGE_LOOP('',(#1033));
#287=EDGE_LOOP('',(#1034,#1035,#1036,#1037,#1038));
#288=EDGE_LOOP('',(#1039,#1040,#1041,#1042));
#289=EDGE_LOOP('',(#1043,#1044,#1045,#1046));
#290=EDGE_LOOP('',(#1047));
#291=EDGE_LOOP('',(#1048));
#292=EDGE_LOOP('',(#1049,#1050,#1051,#1052,#1053));
#293=EDGE_LOOP('',(#1054,#1055,#1056,#1057));
#294=EDGE_LOOP('',(#1058,#1059,#1060,#1061,#1062));
#295=EDGE_LOOP('',(#1063,#1064,#1065,#1066));
#296=EDGE_LOOP('',(#1067,#1068,#1069,#1070,#1071));
#297=EDGE_LOOP('',(#1072,#1073,#1074,#1075));
#298=EDGE_LOOP('',(#1076,#1077,#1078,#1079));
#299=EDGE_LOOP('',(#1080));
#300=EDGE_LOOP('',(#1081));
#301=EDGE_LOOP('',(#1082,#1083,#1084,#1085));
#302=EDGE_LOOP('',(#1086,#1087,#1088,#1089));
#303=EDGE_LOOP('',(#1090,#1091,#1092,#1093));
#304=EDGE_LOOP('',(#1094));
#305=EDGE_LOOP('',(#1095));
#306=EDGE_LOOP('',(#1096,#1097,#1098,#1099));
#307=EDGE_LOOP('',(#1100,#1101,#1102,#1103));
#308=EDGE_LOOP('',(#1104,#1105,#1106,#1107));
#309=EDGE_LOOP('',(#1108,#1109,#1110,#1111));
#310=EDGE_LOOP('',(#1112,#1113,#1114,#1115));
#311=EDGE_LOOP('',(#1116,#1117,#1118,#1119,#1120,#1121));
#312=EDGE_LOOP('',(#1122,#1123,#1124,#1125,#1126,#1127));
#313=EDGE_LOOP('',(#1128,#1129,#1130,#1131,#1132,#1133));
#314=EDGE_LOOP('',(#1134,#1135,#1136,#1137,#1138,#1139));
#315=EDGE_LOOP('',(#1140,#1141,#1142,#1143));
#316=EDGE_LOOP('',(#1144,#1145));
#317=EDGE_LOOP('',(#1146,#1147));
#318=EDGE_LOOP('',(#1148,#1149));
#319=EDGE_LOOP('',(#1150,#1151));
#320=EDGE_LOOP('',(#1152));
#321=EDGE_LOOP('',(#1153,#1154,#1155,#1156));
#322=EDGE_LOOP('',(#1157,#1158));
#323=EDGE_LOOP('',(#1159,#1160));
#324=EDGE_LOOP('',(#1161,#1162));
#325=EDGE_LOOP('',(#1163,#1164));
#326=EDGE_LOOP('',(#1165));
#327=EDGE_LOOP('',(#1166,#1167,#1168,#1169));
#328=EDGE_LOOP('',(#1170));
#329=EDGE_LOOP('',(#1171,#1172,#1173,#1174));
#330=EDGE_LOOP('',(#1175));
#331=EDGE_LOOP('',(#1176,#1177,#1178,#1179));
#332=EDGE_LOOP('',(#1180,#1181,#1182,#1183));
#333=EDGE_LOOP('',(#1184,#1185,#1186,#1187));
#334=EDGE_LOOP('',(#1188,#1189,#1190,#1191));
#335=EDGE_LOOP('',(#1192,#1193,#1194,#1195));
#336=EDGE_LOOP('',(#1196,#1197,#1198,#1199));
#337=EDGE_LOOP('',(#1200,#1201,#1202,#1203));
#338=EDGE_LOOP('',(#1204,#1205,#1206,#1207));
#339=EDGE_LOOP('',(#1208,#1209,#1210,#1211));
#340=EDGE_LOOP('',(#1212,#1213,#1214,#1215));
#341=EDGE_LOOP('',(#1216,#1217,#1218,#1219));
#342=EDGE_LOOP('',(#1220,#1221,#1222,#1223));
#343=EDGE_LOOP('',(#1224,#1225,#1226,#1227));
#344=EDGE_LOOP('',(#1228,#1229,#1230,#1231));
#345=EDGE_LOOP('',(#1232,#1233,#1234,#1235));
#346=EDGE_LOOP('',(#1236,#1237,#1238,#1239));
#347=EDGE_LOOP('',(#1240,#1241,#1242,#1243));
#348=EDGE_LOOP('',(#1244,#1245,#1246,#1247));
#349=EDGE_LOOP('',(#1248,#1249,#1250,#1251));
#350=EDGE_LOOP('',(#1252,#1253,#1254,#1255));
#351=EDGE_LOOP('',(#1256,#1257,#1258,#1259));
#352=EDGE_LOOP('',(#1260,#1261,#1262,#1263));
#353=EDGE_LOOP('',(#1264,#1265,#1266,#1267,#1268,#1269,#1270,#1271,#1272,
#1273,#1274,#1275,#1276,#1277,#1278,#1279));
#354=EDGE_LOOP('',(#1280));
#355=EDGE_LOOP('',(#1281,#1282,#1283,#1284));
#356=EDGE_LOOP('',(#1285,#1286,#1287,#1288));
#357=EDGE_LOOP('',(#1289));
#358=EDGE_LOOP('',(#1290));
#359=EDGE_LOOP('',(#1291));
#360=EDGE_LOOP('',(#1292));
#361=EDGE_LOOP('',(#1293,#1294));
#362=EDGE_LOOP('',(#1295,#1296));
#363=EDGE_LOOP('',(#1297,#1298));
#364=EDGE_LOOP('',(#1299,#1300));
#365=EDGE_LOOP('',(#1301,#1302,#1303,#1304));
#366=EDGE_LOOP('',(#1305,#1306,#1307,#1308,#1309,#1310,#1311,#1312,#1313,
#1314,#1315,#1316,#1317,#1318,#1319,#1320));
#367=EDGE_LOOP('',(#1321));
#368=EDGE_LOOP('',(#1322));
#369=EDGE_LOOP('',(#1323));
#370=EDGE_LOOP('',(#1324));
#371=EDGE_LOOP('',(#1325));
#372=EDGE_LOOP('',(#1326,#1327,#1328,#1329));
#373=EDGE_LOOP('',(#1330,#1331,#1332,#1333));
#374=EDGE_LOOP('',(#1334,#1335,#1336,#1337));
#375=EDGE_LOOP('',(#1338,#1339,#1340,#1341));
#376=EDGE_LOOP('',(#1342,#1343,#1344,#1345));
#377=EDGE_LOOP('',(#1346,#1347,#1348,#1349));
#378=EDGE_LOOP('',(#1350,#1351,#1352,#1353));
#379=EDGE_LOOP('',(#1354,#1355,#1356,#1357));
#380=EDGE_LOOP('',(#1358,#1359,#1360,#1361));
#381=EDGE_LOOP('',(#1362,#1363,#1364,#1365));
#382=EDGE_LOOP('',(#1366,#1367,#1368,#1369));
#383=EDGE_LOOP('',(#1370,#1371,#1372,#1373));
#384=EDGE_LOOP('',(#1374,#1375,#1376,#1377));
#385=EDGE_LOOP('',(#1378,#1379,#1380,#1381));
#386=EDGE_LOOP('',(#1382,#1383,#1384,#1385));
#387=EDGE_LOOP('',(#1386,#1387,#1388,#1389));
#388=EDGE_LOOP('',(#1390,#1391,#1392,#1393));
#389=EDGE_LOOP('',(#1394,#1395,#1396,#1397));
#390=EDGE_LOOP('',(#1398,#1399,#1400,#1401));
#391=EDGE_LOOP('',(#1402,#1403,#1404,#1405));
#392=EDGE_LOOP('',(#1406,#1407,#1408,#1409));
#393=EDGE_LOOP('',(#1410,#1411,#1412,#1413));
#394=EDGE_LOOP('',(#1414,#1415,#1416,#1417));
#395=EDGE_LOOP('',(#1418,#1419,#1420,#1421));
#396=EDGE_LOOP('',(#1422));
#397=EDGE_LOOP('',(#1423,#1424,#1425,#1426));
#398=EDGE_LOOP('',(#1427));
#399=EDGE_LOOP('',(#1428,#1429));
#400=EDGE_LOOP('',(#1430));
#401=EDGE_LOOP('',(#1431,#1432,#1433,#1434));
#402=EDGE_LOOP('',(#1435,#1436,#1437,#1438));
#403=EDGE_LOOP('',(#1439,#1440,#1441,#1442));
#404=EDGE_LOOP('',(#1443));
#405=LINE('',#2311,#502);
#406=LINE('',#2316,#503);
#407=LINE('',#2318,#504);
#408=LINE('',#2320,#505);
#409=LINE('',#2321,#506);
#410=LINE('',#2367,#507);
#411=LINE('',#2372,#508);
#412=LINE('',#2377,#509);
#413=LINE('',#2379,#510);
#414=LINE('',#2381,#511);
#415=LINE('',#2382,#512);
#416=LINE('',#2387,#513);
#417=LINE('',#2431,#514);
#418=LINE('',#2476,#515);
#419=LINE('',#2479,#516);
#420=LINE('',#2483,#517);
#421=LINE('',#2529,#518);
#422=LINE('',#2534,#519);
#423=LINE('',#2536,#520);
#424=LINE('',#2538,#521);
#425=LINE('',#2539,#522);
#426=LINE('',#2578,#523);
#427=LINE('',#2583,#524);
#428=LINE('',#2588,#525);
#429=LINE('',#2590,#526);
#430=LINE('',#2592,#527);
#431=LINE('',#2593,#528);
#432=LINE('',#2598,#529);
#433=LINE('',#2635,#530);
#434=LINE('',#2673,#531);
#435=LINE('',#2676,#532);
#436=LINE('',#2680,#533);
#437=LINE('',#2759,#534);
#438=LINE('',#2837,#535);
#439=LINE('',#2923,#536);
#440=LINE('',#3001,#537);
#441=LINE('',#3047,#538);
#442=LINE('',#3054,#539);
#443=LINE('',#3061,#540);
#444=LINE('',#3068,#541);
#445=LINE('',#3073,#542);
#446=LINE('',#3075,#543);
#447=LINE('',#3076,#544);
#448=LINE('',#3080,#545);
#449=LINE('',#3087,#546);
#450=LINE('',#3091,#547);
#451=LINE('',#3096,#548);
#452=LINE('',#3097,#549);
#453=LINE('',#3101,#550);
#454=LINE('',#3108,#551);
#455=LINE('',#3112,#552);
#456=LINE('',#3117,#553);
#457=LINE('',#3118,#554);
#458=LINE('',#3122,#555);
#459=LINE('',#3129,#556);
#460=LINE('',#3133,#557);
#461=LINE('',#3138,#558);
#462=LINE('',#3139,#559);
#463=LINE('',#3143,#560);
#464=LINE('',#3150,#561);
#465=LINE('',#3157,#562);
#466=LINE('',#3161,#563);
#467=LINE('',#3167,#564);
#468=LINE('',#3171,#565);
#469=LINE('',#3181,#566);
#470=LINE('',#3185,#567);
#471=LINE('',#3189,#568);
#472=LINE('',#3199,#569);
#473=LINE('',#3207,#570);
#474=LINE('',#3215,#571);
#475=LINE('',#3222,#572);
#476=LINE('',#3224,#573);
#477=LINE('',#3225,#574);
#478=LINE('',#3227,#575);
#479=LINE('',#3230,#576);
#480=LINE('',#3234,#577);
#481=LINE('',#3237,#578);
#482=LINE('',#3240,#579);
#483=LINE('',#3243,#580);
#484=LINE('',#3247,#581);
#485=LINE('',#3250,#582);
#486=LINE('',#3253,#583);
#487=LINE('',#3255,#584);
#488=LINE('',#3257,#585);
#489=LINE('',#3259,#586);
#490=LINE('',#3261,#587);
#491=LINE('',#3263,#588);
#492=LINE('',#3266,#589);
#493=LINE('',#3268,#590);
#494=LINE('',#3270,#591);
#495=LINE('',#3272,#592);
#496=LINE('',#3280,#593);
#497=LINE('',#3285,#594);
#498=LINE('',#3290,#595);
#499=LINE('',#3304,#596);
#500=LINE('',#3308,#597);
#501=LINE('',#3312,#598);
#502=VECTOR('',#1826,1.35);
#503=VECTOR('',#1831,10.);
#504=VECTOR('',#1832,10.);
#505=VECTOR('',#1833,10.);
#506=VECTOR('',#1834,10.);
#507=VECTOR('',#1839,1.25);
#508=VECTOR('',#1844,1.35);
#509=VECTOR('',#1849,10.);
#510=VECTOR('',#1850,10.);
#511=VECTOR('',#1851,10.);
#512=VECTOR('',#1852,10.);
#513=VECTOR('',#1857,1.25);
#514=VECTOR('',#1860,1.35);
#515=VECTOR('',#1865,1.25);
#516=VECTOR('',#1868,1.35);
#517=VECTOR('',#1873,1.25);
#518=VECTOR('',#1878,1.35);
#519=VECTOR('',#1883,10.);
#520=VECTOR('',#1884,10.);
#521=VECTOR('',#1885,10.);
#522=VECTOR('',#1886,10.);
#523=VECTOR('',#1891,1.25);
#524=VECTOR('',#1896,1.35);
#525=VECTOR('',#1901,10.);
#526=VECTOR('',#1902,10.);
#527=VECTOR('',#1903,10.);
#528=VECTOR('',#1904,10.);
#529=VECTOR('',#1909,1.25);
#530=VECTOR('',#1912,1.35);
#531=VECTOR('',#1917,1.25);
#532=VECTOR('',#1920,1.35);
#533=VECTOR('',#1925,1.25);
#534=VECTOR('',#1928,1.25);
#535=VECTOR('',#1931,1.25);
#536=VECTOR('',#1934,1.25);
#537=VECTOR('',#1937,1.25);
#538=VECTOR('',#1942,3.5);
#539=VECTOR('',#1951,3.5);
#540=VECTOR('',#1960,5.025);
#541=VECTOR('',#1969,5.025);
#542=VECTOR('',#1976,10.);
#543=VECTOR('',#1977,10.);
#544=VECTOR('',#1978,10.);
#545=VECTOR('',#1981,10.);
#546=VECTOR('',#1990,10.);
#547=VECTOR('',#1995,10.);
#548=VECTOR('',#2002,10.);
#549=VECTOR('',#2003,10.);
#550=VECTOR('',#2006,10.);
#551=VECTOR('',#2015,10.);
#552=VECTOR('',#2020,10.);
#553=VECTOR('',#2027,10.);
#554=VECTOR('',#2028,10.);
#555=VECTOR('',#2031,10.);
#556=VECTOR('',#2040,10.);
#557=VECTOR('',#2045,10.);
#558=VECTOR('',#2052,10.);
#559=VECTOR('',#2053,10.);
#560=VECTOR('',#2056,10.);
#561=VECTOR('',#2065,10.);
#562=VECTOR('',#2076,10.);
#563=VECTOR('',#2081,10.);
#564=VECTOR('',#2090,10.);
#565=VECTOR('',#2095,10.);
#566=VECTOR('',#2110,13.7);
#567=VECTOR('',#2115,13.5);
#568=VECTOR('',#2120,13.9);
#569=VECTOR('',#2129,10.);
#570=VECTOR('',#2136,10.);
#571=VECTOR('',#2143,10.);
#572=VECTOR('',#2150,10.);
#573=VECTOR('',#2153,10.);
#574=VECTOR('',#2154,10.);
#575=VECTOR('',#2157,10.);
#576=VECTOR('',#2160,10.);
#577=VECTOR('',#2165,10.);
#578=VECTOR('',#2170,10.);
#579=VECTOR('',#2175,10.);
#580=VECTOR('',#2178,10.);
#581=VECTOR('',#2183,10.);
#582=VECTOR('',#2188,10.);
#583=VECTOR('',#2193,10.);
#584=VECTOR('',#2196,10.);
#585=VECTOR('',#2199,10.);
#586=VECTOR('',#2202,10.);
#587=VECTOR('',#2205,10.);
#588=VECTOR('',#2208,10.);
#589=VECTOR('',#2213,10.);
#590=VECTOR('',#2216,10.);
#591=VECTOR('',#2219,10.);
#592=VECTOR('',#2222,10.);
#593=VECTOR('',#2233,4.9);
#594=VECTOR('',#2240,5.);
#595=VECTOR('',#2247,4.9);
#596=VECTOR('',#2266,1.125);
#597=VECTOR('',#2271,1.25);
#598=VECTOR('',#2276,1.125);
#599=CIRCLE('',#1626,1.45);
#600=CIRCLE('',#1627,1.25);
#601=CIRCLE('',#1629,1.45);
#602=CIRCLE('',#1632,1.45);
#603=CIRCLE('',#1633,1.25);
#604=CIRCLE('',#1635,1.45);
#605=CIRCLE('',#1638,1.25);
#606=CIRCLE('',#1641,1.25);
#607=CIRCLE('',#1644,1.45);
#608=CIRCLE('',#1645,1.25);
#609=CIRCLE('',#1647,1.45);
#610=CIRCLE('',#1650,1.45);
#611=CIRCLE('',#1651,1.25);
#612=CIRCLE('',#1653,1.45);
#613=CIRCLE('',#1656,1.25);
#614=CIRCLE('',#1659,1.25);
#615=CIRCLE('',#1666,3.5);
#616=CIRCLE('',#1667,3.5);
#617=CIRCLE('',#1670,3.5);
#618=CIRCLE('',#1671,3.5);
#619=CIRCLE('',#1674,5.025);
#620=CIRCLE('',#1675,5.025);
#621=CIRCLE('',#1678,5.025);
#622=CIRCLE('',#1679,5.025);
#623=CIRCLE('',#1683,2.);
#624=CIRCLE('',#1684,1.6);
#625=CIRCLE('',#1686,21.8);
#626=CIRCLE('',#1687,21.4);
#627=CIRCLE('',#1689,2.);
#628=CIRCLE('',#1690,1.6);
#629=CIRCLE('',#1693,2.);
#630=CIRCLE('',#1694,1.6);
#631=CIRCLE('',#1696,21.8);
#632=CIRCLE('',#1697,21.4);
#633=CIRCLE('',#1699,2.);
#634=CIRCLE('',#1700,1.6);
#635=CIRCLE('',#1703,2.);
#636=CIRCLE('',#1704,1.6);
#637=CIRCLE('',#1706,21.8);
#638=CIRCLE('',#1707,21.4);
#639=CIRCLE('',#1709,2.);
#640=CIRCLE('',#1710,1.6);
#641=CIRCLE('',#1713,2.);
#642=CIRCLE('',#1714,1.6);
#643=CIRCLE('',#1716,21.8);
#644=CIRCLE('',#1717,21.4);
#645=CIRCLE('',#1719,2.);
#646=CIRCLE('',#1720,1.6);
#647=CIRCLE('',#1722,2.);
#648=CIRCLE('',#1724,21.4);
#649=CIRCLE('',#1726,2.);
#650=CIRCLE('',#1728,2.);
#651=CIRCLE('',#1730,21.4);
#652=CIRCLE('',#1732,2.);
#653=CIRCLE('',#1734,13.9);
#654=CIRCLE('',#1736,13.5);
#655=CIRCLE('',#1738,13.5);
#656=CIRCLE('',#1740,14.3);
#657=CIRCLE('',#1742,1.2);
#658=CIRCLE('',#1743,22.2);
#659=CIRCLE('',#1744,1.2);
#660=CIRCLE('',#1745,1.2);
#661=CIRCLE('',#1746,22.2);
#662=CIRCLE('',#1747,1.2);
#663=CIRCLE('',#1748,1.2);
#664=CIRCLE('',#1749,22.2);
#665=CIRCLE('',#1750,1.2);
#666=CIRCLE('',#1751,1.2);
#667=CIRCLE('',#1752,22.2);
#668=CIRCLE('',#1753,1.2);
#669=CIRCLE('',#1757,2.);
#670=CIRCLE('',#1759,21.4);
#671=CIRCLE('',#1761,2.);
#672=CIRCLE('',#1764,2.);
#673=CIRCLE('',#1766,21.4);
#674=CIRCLE('',#1768,2.);
#675=CIRCLE('',#1784,5.);
#676=CIRCLE('',#1785,4.8);
#677=CIRCLE('',#1787,5.);
#678=CIRCLE('',#1790,4.8);
#679=CIRCLE('',#1794,2.5);
#680=CIRCLE('',#1797,1.);
#681=CIRCLE('',#1799,1.25);
#682=CIRCLE('',#1801,1.25);
#683=CIRCLE('',#1803,1.);
#684=VERTEX_POINT('',#2308);
#685=VERTEX_POINT('',#2310);
#686=VERTEX_POINT('',#2314);
#687=VERTEX_POINT('',#2315);
#688=VERTEX_POINT('',#2317);
#689=VERTEX_POINT('',#2319);
#690=VERTEX_POINT('',#2322);
#691=VERTEX_POINT('',#2325);
#692=VERTEX_POINT('',#2326);
#693=VERTEX_POINT('',#2369);
#694=VERTEX_POINT('',#2371);
#695=VERTEX_POINT('',#2375);
#696=VERTEX_POINT('',#2376);
#697=VERTEX_POINT('',#2378);
#698=VERTEX_POINT('',#2380);
#699=VERTEX_POINT('',#2383);
#700=VERTEX_POINT('',#2386);
#701=VERTEX_POINT('',#2388);
#702=VERTEX_POINT('',#2430);
#703=VERTEX_POINT('',#2434);
#704=VERTEX_POINT('',#2435);
#705=VERTEX_POINT('',#2478);
#706=VERTEX_POINT('',#2482);
#707=VERTEX_POINT('',#2484);
#708=VERTEX_POINT('',#2526);
#709=VERTEX_POINT('',#2528);
#710=VERTEX_POINT('',#2532);
#711=VERTEX_POINT('',#2533);
#712=VERTEX_POINT('',#2535);
#713=VERTEX_POINT('',#2537);
#714=VERTEX_POINT('',#2540);
#715=VERTEX_POINT('',#2543);
#716=VERTEX_POINT('',#2580);
#717=VERTEX_POINT('',#2582);
#718=VERTEX_POINT('',#2586);
#719=VERTEX_POINT('',#2587);
#720=VERTEX_POINT('',#2589);
#721=VERTEX_POINT('',#2591);
#722=VERTEX_POINT('',#2594);
#723=VERTEX_POINT('',#2597);
#724=VERTEX_POINT('',#2634);
#725=VERTEX_POINT('',#2638);
#726=VERTEX_POINT('',#2675);
#727=VERTEX_POINT('',#2679);
#728=VERTEX_POINT('',#2716);
#729=VERTEX_POINT('',#2717);
#730=VERTEX_POINT('',#2758);
#731=VERTEX_POINT('',#2760);
#732=VERTEX_POINT('',#2798);
#733=VERTEX_POINT('',#2799);
#734=VERTEX_POINT('',#2836);
#735=VERTEX_POINT('',#2838);
#736=VERTEX_POINT('',#2880);
#737=VERTEX_POINT('',#2881);
#738=VERTEX_POINT('',#2922);
#739=VERTEX_POINT('',#2924);
#740=VERTEX_POINT('',#2962);
#741=VERTEX_POINT('',#2963);
#742=VERTEX_POINT('',#3000);
#743=VERTEX_POINT('',#3002);
#744=VERTEX_POINT('',#3044);
#745=VERTEX_POINT('',#3046);
#746=VERTEX_POINT('',#3051);
#747=VERTEX_POINT('',#3053);
#748=VERTEX_POINT('',#3058);
#749=VERTEX_POINT('',#3060);
#750=VERTEX_POINT('',#3065);
#751=VERTEX_POINT('',#3067);
#752=VERTEX_POINT('',#3072);
#753=VERTEX_POINT('',#3074);
#754=VERTEX_POINT('',#3078);
#755=VERTEX_POINT('',#3079);
#756=VERTEX_POINT('',#3084);
#757=VERTEX_POINT('',#3086);
#758=VERTEX_POINT('',#3090);
#759=VERTEX_POINT('',#3095);
#760=VERTEX_POINT('',#3099);
#761=VERTEX_POINT('',#3100);
#762=VERTEX_POINT('',#3105);
#763=VERTEX_POINT('',#3107);
#764=VERTEX_POINT('',#3111);
#765=VERTEX_POINT('',#3116);
#766=VERTEX_POINT('',#3120);
#767=VERTEX_POINT('',#3121);
#768=VERTEX_POINT('',#3126);
#769=VERTEX_POINT('',#3128);
#770=VERTEX_POINT('',#3132);
#771=VERTEX_POINT('',#3137);
#772=VERTEX_POINT('',#3141);
#773=VERTEX_POINT('',#3142);
#774=VERTEX_POINT('',#3147);
#775=VERTEX_POINT('',#3149);
#776=VERTEX_POINT('',#3156);
#777=VERTEX_POINT('',#3160);
#778=VERTEX_POINT('',#3166);
#779=VERTEX_POINT('',#3170);
#780=VERTEX_POINT('',#3176);
#781=VERTEX_POINT('',#3179);
#782=VERTEX_POINT('',#3183);
#783=VERTEX_POINT('',#3187);
#784=VERTEX_POINT('',#3191);
#785=VERTEX_POINT('',#3192);
#786=VERTEX_POINT('',#3194);
#787=VERTEX_POINT('',#3196);
#788=VERTEX_POINT('',#3198);
#789=VERTEX_POINT('',#3200);
#790=VERTEX_POINT('',#3202);
#791=VERTEX_POINT('',#3204);
#792=VERTEX_POINT('',#3206);
#793=VERTEX_POINT('',#3208);
#794=VERTEX_POINT('',#3210);
#795=VERTEX_POINT('',#3212);
#796=VERTEX_POINT('',#3214);
#797=VERTEX_POINT('',#3216);
#798=VERTEX_POINT('',#3218);
#799=VERTEX_POINT('',#3220);
#800=VERTEX_POINT('',#3229);
#801=VERTEX_POINT('',#3233);
#802=VERTEX_POINT('',#3242);
#803=VERTEX_POINT('',#3246);
#804=VERTEX_POINT('',#3277);
#805=VERTEX_POINT('',#3279);
#806=VERTEX_POINT('',#3283);
#807=VERTEX_POINT('',#3288);
#808=VERTEX_POINT('',#3294);
#809=VERTEX_POINT('',#3295);
#810=VERTEX_POINT('',#3299);
#811=VERTEX_POINT('',#3302);
#812=VERTEX_POINT('',#3306);
#813=VERTEX_POINT('',#3310);
#814=EDGE_CURVE('',#684,#684,#599,.T.);
#815=EDGE_CURVE('',#684,#685,#405,.T.);
#816=EDGE_CURVE('',#685,#685,#600,.T.);
#817=EDGE_CURVE('',#686,#687,#406,.T.);
#818=EDGE_CURVE('',#688,#686,#407,.T.);
#819=EDGE_CURVE('',#689,#688,#408,.T.);
#820=EDGE_CURVE('',#687,#689,#409,.T.);
#821=EDGE_CURVE('',#690,#690,#601,.T.);
#822=EDGE_CURVE('',#691,#692,#80,.T.);
#823=EDGE_CURVE('',#692,#691,#81,.T.);
#824=EDGE_CURVE('',#692,#685,#410,.T.);
#825=EDGE_CURVE('',#693,#693,#602,.T.);
#826=EDGE_CURVE('',#693,#694,#411,.T.);
#827=EDGE_CURVE('',#694,#694,#603,.T.);
#828=EDGE_CURVE('',#695,#696,#412,.T.);
#829=EDGE_CURVE('',#697,#695,#413,.T.);
#830=EDGE_CURVE('',#698,#697,#414,.T.);
#831=EDGE_CURVE('',#696,#698,#415,.T.);
#832=EDGE_CURVE('',#699,#699,#604,.T.);
#833=EDGE_CURVE('',#694,#700,#416,.T.);
#834=EDGE_CURVE('',#701,#700,#82,.T.);
#835=EDGE_CURVE('',#700,#701,#83,.T.);
#836=EDGE_CURVE('',#690,#702,#417,.T.);
#837=EDGE_CURVE('',#702,#702,#605,.T.);
#838=EDGE_CURVE('',#703,#704,#84,.T.);
#839=EDGE_CURVE('',#704,#703,#85,.T.);
#840=EDGE_CURVE('',#704,#702,#418,.T.);
#841=EDGE_CURVE('',#699,#705,#419,.T.);
#842=EDGE_CURVE('',#705,#705,#606,.T.);
#843=EDGE_CURVE('',#705,#706,#420,.T.);
#844=EDGE_CURVE('',#707,#706,#86,.T.);
#845=EDGE_CURVE('',#706,#707,#87,.T.);
#846=EDGE_CURVE('',#708,#708,#607,.T.);
#847=EDGE_CURVE('',#708,#709,#421,.T.);
#848=EDGE_CURVE('',#709,#709,#608,.T.);
#849=EDGE_CURVE('',#710,#711,#422,.T.);
#850=EDGE_CURVE('',#712,#710,#423,.T.);
#851=EDGE_CURVE('',#713,#712,#424,.T.);
#852=EDGE_CURVE('',#711,#713,#425,.T.);
#853=EDGE_CURVE('',#714,#714,#609,.T.);
#854=EDGE_CURVE('',#715,#715,#88,.T.);
#855=EDGE_CURVE('',#715,#709,#426,.T.);
#856=EDGE_CURVE('',#716,#716,#610,.T.);
#857=EDGE_CURVE('',#716,#717,#427,.T.);
#858=EDGE_CURVE('',#717,#717,#611,.T.);
#859=EDGE_CURVE('',#718,#719,#428,.T.);
#860=EDGE_CURVE('',#720,#718,#429,.T.);
#861=EDGE_CURVE('',#721,#720,#430,.T.);
#862=EDGE_CURVE('',#719,#721,#431,.T.);
#863=EDGE_CURVE('',#722,#722,#612,.T.);
#864=EDGE_CURVE('',#717,#723,#432,.T.);
#865=EDGE_CURVE('',#723,#723,#89,.T.);
#866=EDGE_CURVE('',#714,#724,#433,.T.);
#867=EDGE_CURVE('',#724,#724,#613,.T.);
#868=EDGE_CURVE('',#725,#725,#90,.T.);
#869=EDGE_CURVE('',#725,#724,#434,.T.);
#870=EDGE_CURVE('',#722,#726,#435,.T.);
#871=EDGE_CURVE('',#726,#726,#614,.T.);
#872=EDGE_CURVE('',#726,#727,#436,.T.);
#873=EDGE_CURVE('',#727,#727,#91,.T.);
#874=EDGE_CURVE('',#728,#729,#92,.T.);
#875=EDGE_CURVE('',#729,#728,#93,.T.);
#876=EDGE_CURVE('',#729,#730,#437,.T.);
#877=EDGE_CURVE('',#731,#730,#94,.T.);
#878=EDGE_CURVE('',#730,#731,#95,.T.);
#879=EDGE_CURVE('',#732,#733,#96,.T.);
#880=EDGE_CURVE('',#733,#732,#97,.T.);
#881=EDGE_CURVE('',#733,#734,#438,.T.);
#882=EDGE_CURVE('',#735,#734,#98,.T.);
#883=EDGE_CURVE('',#734,#735,#99,.T.);
#884=EDGE_CURVE('',#736,#737,#100,.T.);
#885=EDGE_CURVE('',#737,#736,#101,.T.);
#886=EDGE_CURVE('',#737,#738,#439,.T.);
#887=EDGE_CURVE('',#739,#738,#102,.T.);
#888=EDGE_CURVE('',#738,#739,#103,.T.);
#889=EDGE_CURVE('',#740,#741,#104,.T.);
#890=EDGE_CURVE('',#741,#740,#105,.T.);
#891=EDGE_CURVE('',#741,#742,#440,.T.);
#892=EDGE_CURVE('',#743,#742,#106,.T.);
#893=EDGE_CURVE('',#742,#743,#107,.T.);
#894=EDGE_CURVE('',#744,#744,#615,.T.);
#895=EDGE_CURVE('',#744,#745,#441,.T.);
#896=EDGE_CURVE('',#745,#745,#616,.T.);
#897=EDGE_CURVE('',#746,#746,#617,.T.);
#898=EDGE_CURVE('',#746,#747,#442,.T.);
#899=EDGE_CURVE('',#747,#747,#618,.T.);
#900=EDGE_CURVE('',#748,#748,#619,.T.);
#901=EDGE_CURVE('',#748,#749,#443,.T.);
#902=EDGE_CURVE('',#749,#749,#620,.T.);
#903=EDGE_CURVE('',#750,#750,#621,.T.);
#904=EDGE_CURVE('',#750,#751,#444,.T.);
#905=EDGE_CURVE('',#751,#751,#622,.T.);
#906=EDGE_CURVE('',#752,#718,#445,.T.);
#907=EDGE_CURVE('',#719,#753,#446,.T.);
#908=EDGE_CURVE('',#753,#752,#447,.T.);
#909=EDGE_CURVE('',#754,#755,#448,.T.);
#910=EDGE_CURVE('',#755,#718,#623,.T.);
#911=EDGE_CURVE('',#752,#754,#624,.T.);
#912=EDGE_CURVE('',#754,#756,#625,.T.);
#913=EDGE_CURVE('',#756,#757,#449,.T.);
#914=EDGE_CURVE('',#757,#755,#626,.T.);
#915=EDGE_CURVE('',#758,#687,#450,.T.);
#916=EDGE_CURVE('',#687,#757,#627,.T.);
#917=EDGE_CURVE('',#756,#758,#628,.T.);
#918=EDGE_CURVE('',#759,#686,#451,.T.);
#919=EDGE_CURVE('',#758,#759,#452,.T.);
#920=EDGE_CURVE('',#760,#761,#453,.T.);
#921=EDGE_CURVE('',#761,#686,#629,.T.);
#922=EDGE_CURVE('',#759,#760,#630,.T.);
#923=EDGE_CURVE('',#760,#762,#631,.T.);
#924=EDGE_CURVE('',#762,#763,#454,.T.);
#925=EDGE_CURVE('',#763,#761,#632,.T.);
#926=EDGE_CURVE('',#764,#711,#455,.T.);
#927=EDGE_CURVE('',#711,#763,#633,.T.);
#928=EDGE_CURVE('',#762,#764,#634,.T.);
#929=EDGE_CURVE('',#765,#710,#456,.T.);
#930=EDGE_CURVE('',#764,#765,#457,.T.);
#931=EDGE_CURVE('',#766,#767,#458,.T.);
#932=EDGE_CURVE('',#767,#710,#635,.T.);
#933=EDGE_CURVE('',#765,#766,#636,.T.);
#934=EDGE_CURVE('',#766,#768,#637,.T.);
#935=EDGE_CURVE('',#768,#769,#459,.T.);
#936=EDGE_CURVE('',#769,#767,#638,.T.);
#937=EDGE_CURVE('',#770,#696,#460,.T.);
#938=EDGE_CURVE('',#696,#769,#639,.T.);
#939=EDGE_CURVE('',#768,#770,#640,.T.);
#940=EDGE_CURVE('',#771,#695,#461,.T.);
#941=EDGE_CURVE('',#770,#771,#462,.T.);
#942=EDGE_CURVE('',#772,#773,#463,.T.);
#943=EDGE_CURVE('',#773,#695,#641,.T.);
#944=EDGE_CURVE('',#771,#772,#642,.T.);
#945=EDGE_CURVE('',#772,#774,#643,.T.);
#946=EDGE_CURVE('',#774,#775,#464,.T.);
#947=EDGE_CURVE('',#775,#773,#644,.T.);
#948=EDGE_CURVE('',#719,#775,#645,.T.);
#949=EDGE_CURVE('',#774,#753,#646,.T.);
#950=EDGE_CURVE('',#767,#776,#465,.T.);
#951=EDGE_CURVE('',#712,#776,#647,.T.);
#952=EDGE_CURVE('',#777,#769,#466,.T.);
#953=EDGE_CURVE('',#776,#777,#648,.T.);
#954=EDGE_CURVE('',#777,#698,#649,.T.);
#955=EDGE_CURVE('',#773,#778,#467,.T.);
#956=EDGE_CURVE('',#697,#778,#650,.T.);
#957=EDGE_CURVE('',#779,#775,#468,.T.);
#958=EDGE_CURVE('',#778,#779,#651,.T.);
#959=EDGE_CURVE('',#779,#721,#652,.T.);
#960=EDGE_CURVE('',#780,#780,#653,.T.);
#961=EDGE_CURVE('',#781,#781,#654,.T.);
#962=EDGE_CURVE('',#781,#780,#469,.T.);
#963=EDGE_CURVE('',#782,#782,#655,.T.);
#964=EDGE_CURVE('',#782,#781,#470,.T.);
#965=EDGE_CURVE('',#783,#783,#656,.T.);
#966=EDGE_CURVE('',#783,#782,#471,.T.);
#967=EDGE_CURVE('',#784,#785,#657,.T.);
#968=EDGE_CURVE('',#786,#784,#658,.T.);
#969=EDGE_CURVE('',#787,#786,#659,.T.);
#970=EDGE_CURVE('',#788,#787,#472,.T.);
#971=EDGE_CURVE('',#789,#788,#660,.T.);
#972=EDGE_CURVE('',#790,#789,#661,.T.);
#973=EDGE_CURVE('',#791,#790,#662,.T.);
#974=EDGE_CURVE('',#792,#791,#473,.T.);
#975=EDGE_CURVE('',#793,#792,#663,.T.);
#976=EDGE_CURVE('',#794,#793,#664,.T.);
#977=EDGE_CURVE('',#795,#794,#665,.T.);
#978=EDGE_CURVE('',#796,#795,#474,.T.);
#979=EDGE_CURVE('',#797,#796,#666,.T.);
#980=EDGE_CURVE('',#798,#797,#667,.T.);
#981=EDGE_CURVE('',#799,#798,#668,.T.);
#982=EDGE_CURVE('',#785,#799,#475,.T.);
#983=EDGE_CURVE('',#785,#712,#476,.T.);
#984=EDGE_CURVE('',#776,#784,#477,.T.);
#985=EDGE_CURVE('',#799,#713,#478,.T.);
#986=EDGE_CURVE('',#798,#800,#479,.T.);
#987=EDGE_CURVE('',#800,#713,#669,.T.);
#988=EDGE_CURVE('',#797,#801,#480,.T.);
#989=EDGE_CURVE('',#801,#800,#670,.T.);
#990=EDGE_CURVE('',#796,#688,#481,.T.);
#991=EDGE_CURVE('',#688,#801,#671,.T.);
#992=EDGE_CURVE('',#795,#689,#482,.T.);
#993=EDGE_CURVE('',#794,#802,#483,.T.);
#994=EDGE_CURVE('',#802,#689,#672,.T.);
#995=EDGE_CURVE('',#793,#803,#484,.T.);
#996=EDGE_CURVE('',#803,#802,#673,.T.);
#997=EDGE_CURVE('',#792,#720,#485,.T.);
#998=EDGE_CURVE('',#720,#803,#674,.T.);
#999=EDGE_CURVE('',#791,#721,#486,.T.);
#1000=EDGE_CURVE('',#790,#779,#487,.T.);
#1001=EDGE_CURVE('',#789,#778,#488,.T.);
#1002=EDGE_CURVE('',#788,#697,#489,.T.);
#1003=EDGE_CURVE('',#787,#698,#490,.T.);
#1004=EDGE_CURVE('',#786,#777,#491,.T.);
#1005=EDGE_CURVE('',#755,#803,#492,.T.);
#1006=EDGE_CURVE('',#802,#757,#493,.T.);
#1007=EDGE_CURVE('',#761,#801,#494,.T.);
#1008=EDGE_CURVE('',#800,#763,#495,.T.);
#1009=EDGE_CURVE('',#804,#804,#675,.T.);
#1010=EDGE_CURVE('',#804,#805,#496,.T.);
#1011=EDGE_CURVE('',#805,#805,#676,.T.);
#1012=EDGE_CURVE('',#806,#806,#677,.T.);
#1013=EDGE_CURVE('',#806,#804,#497,.T.);
#1014=EDGE_CURVE('',#807,#807,#678,.T.);
#1015=EDGE_CURVE('',#807,#806,#498,.T.);
#1016=EDGE_CURVE('',#808,#809,#679,.T.);
#1017=EDGE_CURVE('',#810,#810,#680,.T.);
#1018=EDGE_CURVE('',#811,#811,#681,.T.);
#1019=EDGE_CURVE('',#811,#810,#499,.T.);
#1020=EDGE_CURVE('',#812,#812,#682,.T.);
#1021=EDGE_CURVE('',#812,#811,#500,.T.);
#1022=EDGE_CURVE('',#813,#813,#683,.T.);
#1023=EDGE_CURVE('',#813,#812,#501,.T.);
#1024=ORIENTED_EDGE('',*,*,#814,.T.);
#1025=ORIENTED_EDGE('',*,*,#815,.T.);
#1026=ORIENTED_EDGE('',*,*,#816,.T.);
#1027=ORIENTED_EDGE('',*,*,#815,.F.);
#1028=ORIENTED_EDGE('',*,*,#817,.F.);
#1029=ORIENTED_EDGE('',*,*,#818,.F.);
#1030=ORIENTED_EDGE('',*,*,#819,.F.);
#1031=ORIENTED_EDGE('',*,*,#820,.F.);
#1032=ORIENTED_EDGE('',*,*,#821,.F.);
#1033=ORIENTED_EDGE('',*,*,#814,.F.);
#1034=ORIENTED_EDGE('',*,*,#822,.F.);
#1035=ORIENTED_EDGE('',*,*,#823,.F.);
#1036=ORIENTED_EDGE('',*,*,#824,.T.);
#1037=ORIENTED_EDGE('',*,*,#816,.F.);
#1038=ORIENTED_EDGE('',*,*,#824,.F.);
#1039=ORIENTED_EDGE('',*,*,#825,.T.);
#1040=ORIENTED_EDGE('',*,*,#826,.T.);
#1041=ORIENTED_EDGE('',*,*,#827,.T.);
#1042=ORIENTED_EDGE('',*,*,#826,.F.);
#1043=ORIENTED_EDGE('',*,*,#828,.F.);
#1044=ORIENTED_EDGE('',*,*,#829,.F.);
#1045=ORIENTED_EDGE('',*,*,#830,.F.);
#1046=ORIENTED_EDGE('',*,*,#831,.F.);
#1047=ORIENTED_EDGE('',*,*,#832,.F.);
#1048=ORIENTED_EDGE('',*,*,#825,.F.);
#1049=ORIENTED_EDGE('',*,*,#827,.F.);
#1050=ORIENTED_EDGE('',*,*,#833,.T.);
#1051=ORIENTED_EDGE('',*,*,#834,.F.);
#1052=ORIENTED_EDGE('',*,*,#835,.F.);
#1053=ORIENTED_EDGE('',*,*,#833,.F.);
#1054=ORIENTED_EDGE('',*,*,#821,.T.);
#1055=ORIENTED_EDGE('',*,*,#836,.T.);
#1056=ORIENTED_EDGE('',*,*,#837,.T.);
#1057=ORIENTED_EDGE('',*,*,#836,.F.);
#1058=ORIENTED_EDGE('',*,*,#838,.F.);
#1059=ORIENTED_EDGE('',*,*,#839,.F.);
#1060=ORIENTED_EDGE('',*,*,#840,.T.);
#1061=ORIENTED_EDGE('',*,*,#837,.F.);
#1062=ORIENTED_EDGE('',*,*,#840,.F.);
#1063=ORIENTED_EDGE('',*,*,#832,.T.);
#1064=ORIENTED_EDGE('',*,*,#841,.T.);
#1065=ORIENTED_EDGE('',*,*,#842,.T.);
#1066=ORIENTED_EDGE('',*,*,#841,.F.);
#1067=ORIENTED_EDGE('',*,*,#842,.F.);
#1068=ORIENTED_EDGE('',*,*,#843,.T.);
#1069=ORIENTED_EDGE('',*,*,#844,.F.);
#1070=ORIENTED_EDGE('',*,*,#845,.F.);
#1071=ORIENTED_EDGE('',*,*,#843,.F.);
#1072=ORIENTED_EDGE('',*,*,#846,.T.);
#1073=ORIENTED_EDGE('',*,*,#847,.T.);
#1074=ORIENTED_EDGE('',*,*,#848,.T.);
#1075=ORIENTED_EDGE('',*,*,#847,.F.);
#1076=ORIENTED_EDGE('',*,*,#849,.F.);
#1077=ORIENTED_EDGE('',*,*,#850,.F.);
#1078=ORIENTED_EDGE('',*,*,#851,.F.);
#1079=ORIENTED_EDGE('',*,*,#852,.F.);
#1080=ORIENTED_EDGE('',*,*,#853,.F.);
#1081=ORIENTED_EDGE('',*,*,#846,.F.);
#1082=ORIENTED_EDGE('',*,*,#854,.F.);
#1083=ORIENTED_EDGE('',*,*,#855,.T.);
#1084=ORIENTED_EDGE('',*,*,#848,.F.);
#1085=ORIENTED_EDGE('',*,*,#855,.F.);
#1086=ORIENTED_EDGE('',*,*,#856,.T.);
#1087=ORIENTED_EDGE('',*,*,#857,.T.);
#1088=ORIENTED_EDGE('',*,*,#858,.T.);
#1089=ORIENTED_EDGE('',*,*,#857,.F.);
#1090=ORIENTED_EDGE('',*,*,#859,.F.);
#1091=ORIENTED_EDGE('',*,*,#860,.F.);
#1092=ORIENTED_EDGE('',*,*,#861,.F.);
#1093=ORIENTED_EDGE('',*,*,#862,.F.);
#1094=ORIENTED_EDGE('',*,*,#863,.F.);
#1095=ORIENTED_EDGE('',*,*,#856,.F.);
#1096=ORIENTED_EDGE('',*,*,#858,.F.);
#1097=ORIENTED_EDGE('',*,*,#864,.T.);
#1098=ORIENTED_EDGE('',*,*,#865,.F.);
#1099=ORIENTED_EDGE('',*,*,#864,.F.);
#1100=ORIENTED_EDGE('',*,*,#853,.T.);
#1101=ORIENTED_EDGE('',*,*,#866,.T.);
#1102=ORIENTED_EDGE('',*,*,#867,.T.);
#1103=ORIENTED_EDGE('',*,*,#866,.F.);
#1104=ORIENTED_EDGE('',*,*,#868,.F.);
#1105=ORIENTED_EDGE('',*,*,#869,.T.);
#1106=ORIENTED_EDGE('',*,*,#867,.F.);
#1107=ORIENTED_EDGE('',*,*,#869,.F.);
#1108=ORIENTED_EDGE('',*,*,#863,.T.);
#1109=ORIENTED_EDGE('',*,*,#870,.T.);
#1110=ORIENTED_EDGE('',*,*,#871,.T.);
#1111=ORIENTED_EDGE('',*,*,#870,.F.);
#1112=ORIENTED_EDGE('',*,*,#871,.F.);
#1113=ORIENTED_EDGE('',*,*,#872,.T.);
#1114=ORIENTED_EDGE('',*,*,#873,.F.);
#1115=ORIENTED_EDGE('',*,*,#872,.F.);
#1116=ORIENTED_EDGE('',*,*,#874,.F.);
#1117=ORIENTED_EDGE('',*,*,#875,.F.);
#1118=ORIENTED_EDGE('',*,*,#876,.T.);
#1119=ORIENTED_EDGE('',*,*,#877,.F.);
#1120=ORIENTED_EDGE('',*,*,#878,.F.);
#1121=ORIENTED_EDGE('',*,*,#876,.F.);
#1122=ORIENTED_EDGE('',*,*,#879,.F.);
#1123=ORIENTED_EDGE('',*,*,#880,.F.);
#1124=ORIENTED_EDGE('',*,*,#881,.T.);
#1125=ORIENTED_EDGE('',*,*,#882,.F.);
#1126=ORIENTED_EDGE('',*,*,#883,.F.);
#1127=ORIENTED_EDGE('',*,*,#881,.F.);
#1128=ORIENTED_EDGE('',*,*,#884,.F.);
#1129=ORIENTED_EDGE('',*,*,#885,.F.);
#1130=ORIENTED_EDGE('',*,*,#886,.T.);
#1131=ORIENTED_EDGE('',*,*,#887,.F.);
#1132=ORIENTED_EDGE('',*,*,#888,.F.);
#1133=ORIENTED_EDGE('',*,*,#886,.F.);
#1134=ORIENTED_EDGE('',*,*,#889,.F.);
#1135=ORIENTED_EDGE('',*,*,#890,.F.);
#1136=ORIENTED_EDGE('',*,*,#891,.T.);
#1137=ORIENTED_EDGE('',*,*,#892,.F.);
#1138=ORIENTED_EDGE('',*,*,#893,.F.);
#1139=ORIENTED_EDGE('',*,*,#891,.F.);
#1140=ORIENTED_EDGE('',*,*,#894,.F.);
#1141=ORIENTED_EDGE('',*,*,#895,.T.);
#1142=ORIENTED_EDGE('',*,*,#896,.F.);
#1143=ORIENTED_EDGE('',*,*,#895,.F.);
#1144=ORIENTED_EDGE('',*,*,#838,.T.);
#1145=ORIENTED_EDGE('',*,*,#839,.T.);
#1146=ORIENTED_EDGE('',*,*,#882,.T.);
#1147=ORIENTED_EDGE('',*,*,#883,.T.);
#1148=ORIENTED_EDGE('',*,*,#822,.T.);
#1149=ORIENTED_EDGE('',*,*,#823,.T.);
#1150=ORIENTED_EDGE('',*,*,#892,.T.);
#1151=ORIENTED_EDGE('',*,*,#893,.T.);
#1152=ORIENTED_EDGE('',*,*,#894,.T.);
#1153=ORIENTED_EDGE('',*,*,#897,.F.);
#1154=ORIENTED_EDGE('',*,*,#898,.T.);
#1155=ORIENTED_EDGE('',*,*,#899,.F.);
#1156=ORIENTED_EDGE('',*,*,#898,.F.);
#1157=ORIENTED_EDGE('',*,*,#874,.T.);
#1158=ORIENTED_EDGE('',*,*,#875,.T.);
#1159=ORIENTED_EDGE('',*,*,#844,.T.);
#1160=ORIENTED_EDGE('',*,*,#845,.T.);
#1161=ORIENTED_EDGE('',*,*,#884,.T.);
#1162=ORIENTED_EDGE('',*,*,#885,.T.);
#1163=ORIENTED_EDGE('',*,*,#834,.T.);
#1164=ORIENTED_EDGE('',*,*,#835,.T.);
#1165=ORIENTED_EDGE('',*,*,#897,.T.);
#1166=ORIENTED_EDGE('',*,*,#900,.F.);
#1167=ORIENTED_EDGE('',*,*,#901,.T.);
#1168=ORIENTED_EDGE('',*,*,#902,.F.);
#1169=ORIENTED_EDGE('',*,*,#901,.F.);
#1170=ORIENTED_EDGE('',*,*,#900,.T.);
#1171=ORIENTED_EDGE('',*,*,#903,.F.);
#1172=ORIENTED_EDGE('',*,*,#904,.T.);
#1173=ORIENTED_EDGE('',*,*,#905,.F.);
#1174=ORIENTED_EDGE('',*,*,#904,.F.);
#1175=ORIENTED_EDGE('',*,*,#903,.T.);
#1176=ORIENTED_EDGE('',*,*,#906,.T.);
#1177=ORIENTED_EDGE('',*,*,#859,.T.);
#1178=ORIENTED_EDGE('',*,*,#907,.T.);
#1179=ORIENTED_EDGE('',*,*,#908,.T.);
#1180=ORIENTED_EDGE('',*,*,#909,.T.);
#1181=ORIENTED_EDGE('',*,*,#910,.T.);
#1182=ORIENTED_EDGE('',*,*,#906,.F.);
#1183=ORIENTED_EDGE('',*,*,#911,.T.);
#1184=ORIENTED_EDGE('',*,*,#909,.F.);
#1185=ORIENTED_EDGE('',*,*,#912,.T.);
#1186=ORIENTED_EDGE('',*,*,#913,.T.);
#1187=ORIENTED_EDGE('',*,*,#914,.T.);
#1188=ORIENTED_EDGE('',*,*,#915,.T.);
#1189=ORIENTED_EDGE('',*,*,#916,.T.);
#1190=ORIENTED_EDGE('',*,*,#913,.F.);
#1191=ORIENTED_EDGE('',*,*,#917,.T.);
#1192=ORIENTED_EDGE('',*,*,#918,.T.);
#1193=ORIENTED_EDGE('',*,*,#817,.T.);
#1194=ORIENTED_EDGE('',*,*,#915,.F.);
#1195=ORIENTED_EDGE('',*,*,#919,.T.);
#1196=ORIENTED_EDGE('',*,*,#920,.T.);
#1197=ORIENTED_EDGE('',*,*,#921,.T.);
#1198=ORIENTED_EDGE('',*,*,#918,.F.);
#1199=ORIENTED_EDGE('',*,*,#922,.T.);
#1200=ORIENTED_EDGE('',*,*,#920,.F.);
#1201=ORIENTED_EDGE('',*,*,#923,.T.);
#1202=ORIENTED_EDGE('',*,*,#924,.T.);
#1203=ORIENTED_EDGE('',*,*,#925,.T.);
#1204=ORIENTED_EDGE('',*,*,#926,.T.);
#1205=ORIENTED_EDGE('',*,*,#927,.T.);
#1206=ORIENTED_EDGE('',*,*,#924,.F.);
#1207=ORIENTED_EDGE('',*,*,#928,.T.);
#1208=ORIENTED_EDGE('',*,*,#929,.T.);
#1209=ORIENTED_EDGE('',*,*,#849,.T.);
#1210=ORIENTED_EDGE('',*,*,#926,.F.);
#1211=ORIENTED_EDGE('',*,*,#930,.T.);
#1212=ORIENTED_EDGE('',*,*,#931,.T.);
#1213=ORIENTED_EDGE('',*,*,#932,.T.);
#1214=ORIENTED_EDGE('',*,*,#929,.F.);
#1215=ORIENTED_EDGE('',*,*,#933,.T.);
#1216=ORIENTED_EDGE('',*,*,#931,.F.);
#1217=ORIENTED_EDGE('',*,*,#934,.T.);
#1218=ORIENTED_EDGE('',*,*,#935,.T.);
#1219=ORIENTED_EDGE('',*,*,#936,.T.);
#1220=ORIENTED_EDGE('',*,*,#937,.T.);
#1221=ORIENTED_EDGE('',*,*,#938,.T.);
#1222=ORIENTED_EDGE('',*,*,#935,.F.);
#1223=ORIENTED_EDGE('',*,*,#939,.T.);
#1224=ORIENTED_EDGE('',*,*,#940,.T.);
#1225=ORIENTED_EDGE('',*,*,#828,.T.);
#1226=ORIENTED_EDGE('',*,*,#937,.F.);
#1227=ORIENTED_EDGE('',*,*,#941,.T.);
#1228=ORIENTED_EDGE('',*,*,#942,.T.);
#1229=ORIENTED_EDGE('',*,*,#943,.T.);
#1230=ORIENTED_EDGE('',*,*,#940,.F.);
#1231=ORIENTED_EDGE('',*,*,#944,.T.);
#1232=ORIENTED_EDGE('',*,*,#942,.F.);
#1233=ORIENTED_EDGE('',*,*,#945,.T.);
#1234=ORIENTED_EDGE('',*,*,#946,.T.);
#1235=ORIENTED_EDGE('',*,*,#947,.T.);
#1236=ORIENTED_EDGE('',*,*,#907,.F.);
#1237=ORIENTED_EDGE('',*,*,#948,.T.);
#1238=ORIENTED_EDGE('',*,*,#946,.F.);
#1239=ORIENTED_EDGE('',*,*,#949,.T.);
#1240=ORIENTED_EDGE('',*,*,#932,.F.);
#1241=ORIENTED_EDGE('',*,*,#950,.T.);
#1242=ORIENTED_EDGE('',*,*,#951,.F.);
#1243=ORIENTED_EDGE('',*,*,#850,.T.);
#1244=ORIENTED_EDGE('',*,*,#936,.F.);
#1245=ORIENTED_EDGE('',*,*,#952,.F.);
#1246=ORIENTED_EDGE('',*,*,#953,.F.);
#1247=ORIENTED_EDGE('',*,*,#950,.F.);
#1248=ORIENTED_EDGE('',*,*,#938,.F.);
#1249=ORIENTED_EDGE('',*,*,#831,.T.);
#1250=ORIENTED_EDGE('',*,*,#954,.F.);
#1251=ORIENTED_EDGE('',*,*,#952,.T.);
#1252=ORIENTED_EDGE('',*,*,#943,.F.);
#1253=ORIENTED_EDGE('',*,*,#955,.T.);
#1254=ORIENTED_EDGE('',*,*,#956,.F.);
#1255=ORIENTED_EDGE('',*,*,#829,.T.);
#1256=ORIENTED_EDGE('',*,*,#947,.F.);
#1257=ORIENTED_EDGE('',*,*,#957,.F.);
#1258=ORIENTED_EDGE('',*,*,#958,.F.);
#1259=ORIENTED_EDGE('',*,*,#955,.F.);
#1260=ORIENTED_EDGE('',*,*,#948,.F.);
#1261=ORIENTED_EDGE('',*,*,#862,.T.);
#1262=ORIENTED_EDGE('',*,*,#959,.F.);
#1263=ORIENTED_EDGE('',*,*,#957,.T.);
#1264=ORIENTED_EDGE('',*,*,#908,.F.);
#1265=ORIENTED_EDGE('',*,*,#949,.F.);
#1266=ORIENTED_EDGE('',*,*,#945,.F.);
#1267=ORIENTED_EDGE('',*,*,#944,.F.);
#1268=ORIENTED_EDGE('',*,*,#941,.F.);
#1269=ORIENTED_EDGE('',*,*,#939,.F.);
#1270=ORIENTED_EDGE('',*,*,#934,.F.);
#1271=ORIENTED_EDGE('',*,*,#933,.F.);
#1272=ORIENTED_EDGE('',*,*,#930,.F.);
#1273=ORIENTED_EDGE('',*,*,#928,.F.);
#1274=ORIENTED_EDGE('',*,*,#923,.F.);
#1275=ORIENTED_EDGE('',*,*,#922,.F.);
#1276=ORIENTED_EDGE('',*,*,#919,.F.);
#1277=ORIENTED_EDGE('',*,*,#917,.F.);
#1278=ORIENTED_EDGE('',*,*,#912,.F.);
#1279=ORIENTED_EDGE('',*,*,#911,.F.);
#1280=ORIENTED_EDGE('',*,*,#960,.F.);
#1281=ORIENTED_EDGE('',*,*,#961,.T.);
#1282=ORIENTED_EDGE('',*,*,#962,.T.);
#1283=ORIENTED_EDGE('',*,*,#960,.T.);
#1284=ORIENTED_EDGE('',*,*,#962,.F.);
#1285=ORIENTED_EDGE('',*,*,#963,.F.);
#1286=ORIENTED_EDGE('',*,*,#964,.T.);
#1287=ORIENTED_EDGE('',*,*,#961,.F.);
#1288=ORIENTED_EDGE('',*,*,#964,.F.);
#1289=ORIENTED_EDGE('',*,*,#868,.T.);
#1290=ORIENTED_EDGE('',*,*,#873,.T.);
#1291=ORIENTED_EDGE('',*,*,#854,.T.);
#1292=ORIENTED_EDGE('',*,*,#865,.T.);
#1293=ORIENTED_EDGE('',*,*,#879,.T.);
#1294=ORIENTED_EDGE('',*,*,#880,.T.);
#1295=ORIENTED_EDGE('',*,*,#877,.T.);
#1296=ORIENTED_EDGE('',*,*,#878,.T.);
#1297=ORIENTED_EDGE('',*,*,#889,.T.);
#1298=ORIENTED_EDGE('',*,*,#890,.T.);
#1299=ORIENTED_EDGE('',*,*,#887,.T.);
#1300=ORIENTED_EDGE('',*,*,#888,.T.);
#1301=ORIENTED_EDGE('',*,*,#965,.T.);
#1302=ORIENTED_EDGE('',*,*,#966,.T.);
#1303=ORIENTED_EDGE('',*,*,#963,.T.);
#1304=ORIENTED_EDGE('',*,*,#966,.F.);
#1305=ORIENTED_EDGE('',*,*,#967,.F.);
#1306=ORIENTED_EDGE('',*,*,#968,.F.);
#1307=ORIENTED_EDGE('',*,*,#969,.F.);
#1308=ORIENTED_EDGE('',*,*,#970,.F.);
#1309=ORIENTED_EDGE('',*,*,#971,.F.);
#1310=ORIENTED_EDGE('',*,*,#972,.F.);
#1311=ORIENTED_EDGE('',*,*,#973,.F.);
#1312=ORIENTED_EDGE('',*,*,#974,.F.);
#1313=ORIENTED_EDGE('',*,*,#975,.F.);
#1314=ORIENTED_EDGE('',*,*,#976,.F.);
#1315=ORIENTED_EDGE('',*,*,#977,.F.);
#1316=ORIENTED_EDGE('',*,*,#978,.F.);
#1317=ORIENTED_EDGE('',*,*,#979,.F.);
#1318=ORIENTED_EDGE('',*,*,#980,.F.);
#1319=ORIENTED_EDGE('',*,*,#981,.F.);
#1320=ORIENTED_EDGE('',*,*,#982,.F.);
#1321=ORIENTED_EDGE('',*,*,#896,.T.);
#1322=ORIENTED_EDGE('',*,*,#899,.T.);
#1323=ORIENTED_EDGE('',*,*,#902,.T.);
#1324=ORIENTED_EDGE('',*,*,#905,.T.);
#1325=ORIENTED_EDGE('',*,*,#965,.F.);
#1326=ORIENTED_EDGE('',*,*,#983,.T.);
#1327=ORIENTED_EDGE('',*,*,#951,.T.);
#1328=ORIENTED_EDGE('',*,*,#984,.T.);
#1329=ORIENTED_EDGE('',*,*,#967,.T.);
#1330=ORIENTED_EDGE('',*,*,#983,.F.);
#1331=ORIENTED_EDGE('',*,*,#982,.T.);
#1332=ORIENTED_EDGE('',*,*,#985,.T.);
#1333=ORIENTED_EDGE('',*,*,#851,.T.);
#1334=ORIENTED_EDGE('',*,*,#986,.T.);
#1335=ORIENTED_EDGE('',*,*,#987,.T.);
#1336=ORIENTED_EDGE('',*,*,#985,.F.);
#1337=ORIENTED_EDGE('',*,*,#981,.T.);
#1338=ORIENTED_EDGE('',*,*,#986,.F.);
#1339=ORIENTED_EDGE('',*,*,#980,.T.);
#1340=ORIENTED_EDGE('',*,*,#988,.T.);
#1341=ORIENTED_EDGE('',*,*,#989,.T.);
#1342=ORIENTED_EDGE('',*,*,#990,.T.);
#1343=ORIENTED_EDGE('',*,*,#991,.T.);
#1344=ORIENTED_EDGE('',*,*,#988,.F.);
#1345=ORIENTED_EDGE('',*,*,#979,.T.);
#1346=ORIENTED_EDGE('',*,*,#990,.F.);
#1347=ORIENTED_EDGE('',*,*,#978,.T.);
#1348=ORIENTED_EDGE('',*,*,#992,.T.);
#1349=ORIENTED_EDGE('',*,*,#819,.T.);
#1350=ORIENTED_EDGE('',*,*,#993,.T.);
#1351=ORIENTED_EDGE('',*,*,#994,.T.);
#1352=ORIENTED_EDGE('',*,*,#992,.F.);
#1353=ORIENTED_EDGE('',*,*,#977,.T.);
#1354=ORIENTED_EDGE('',*,*,#993,.F.);
#1355=ORIENTED_EDGE('',*,*,#976,.T.);
#1356=ORIENTED_EDGE('',*,*,#995,.T.);
#1357=ORIENTED_EDGE('',*,*,#996,.T.);
#1358=ORIENTED_EDGE('',*,*,#997,.T.);
#1359=ORIENTED_EDGE('',*,*,#998,.T.);
#1360=ORIENTED_EDGE('',*,*,#995,.F.);
#1361=ORIENTED_EDGE('',*,*,#975,.T.);
#1362=ORIENTED_EDGE('',*,*,#997,.F.);
#1363=ORIENTED_EDGE('',*,*,#974,.T.);
#1364=ORIENTED_EDGE('',*,*,#999,.T.);
#1365=ORIENTED_EDGE('',*,*,#861,.T.);
#1366=ORIENTED_EDGE('',*,*,#1000,.T.);
#1367=ORIENTED_EDGE('',*,*,#959,.T.);
#1368=ORIENTED_EDGE('',*,*,#999,.F.);
#1369=ORIENTED_EDGE('',*,*,#973,.T.);
#1370=ORIENTED_EDGE('',*,*,#1000,.F.);
#1371=ORIENTED_EDGE('',*,*,#972,.T.);
#1372=ORIENTED_EDGE('',*,*,#1001,.T.);
#1373=ORIENTED_EDGE('',*,*,#958,.T.);
#1374=ORIENTED_EDGE('',*,*,#1002,.T.);
#1375=ORIENTED_EDGE('',*,*,#956,.T.);
#1376=ORIENTED_EDGE('',*,*,#1001,.F.);
#1377=ORIENTED_EDGE('',*,*,#971,.T.);
#1378=ORIENTED_EDGE('',*,*,#1002,.F.);
#1379=ORIENTED_EDGE('',*,*,#970,.T.);
#1380=ORIENTED_EDGE('',*,*,#1003,.T.);
#1381=ORIENTED_EDGE('',*,*,#830,.T.);
#1382=ORIENTED_EDGE('',*,*,#1004,.T.);
#1383=ORIENTED_EDGE('',*,*,#954,.T.);
#1384=ORIENTED_EDGE('',*,*,#1003,.F.);
#1385=ORIENTED_EDGE('',*,*,#969,.T.);
#1386=ORIENTED_EDGE('',*,*,#1004,.F.);
#1387=ORIENTED_EDGE('',*,*,#968,.T.);
#1388=ORIENTED_EDGE('',*,*,#984,.F.);
#1389=ORIENTED_EDGE('',*,*,#953,.T.);
#1390=ORIENTED_EDGE('',*,*,#910,.F.);
#1391=ORIENTED_EDGE('',*,*,#1005,.T.);
#1392=ORIENTED_EDGE('',*,*,#998,.F.);
#1393=ORIENTED_EDGE('',*,*,#860,.T.);
#1394=ORIENTED_EDGE('',*,*,#916,.F.);
#1395=ORIENTED_EDGE('',*,*,#820,.T.);
#1396=ORIENTED_EDGE('',*,*,#994,.F.);
#1397=ORIENTED_EDGE('',*,*,#1006,.T.);
#1398=ORIENTED_EDGE('',*,*,#921,.F.);
#1399=ORIENTED_EDGE('',*,*,#1007,.T.);
#1400=ORIENTED_EDGE('',*,*,#991,.F.);
#1401=ORIENTED_EDGE('',*,*,#818,.T.);
#1402=ORIENTED_EDGE('',*,*,#927,.F.);
#1403=ORIENTED_EDGE('',*,*,#852,.T.);
#1404=ORIENTED_EDGE('',*,*,#987,.F.);
#1405=ORIENTED_EDGE('',*,*,#1008,.T.);
#1406=ORIENTED_EDGE('',*,*,#925,.F.);
#1407=ORIENTED_EDGE('',*,*,#1008,.F.);
#1408=ORIENTED_EDGE('',*,*,#989,.F.);
#1409=ORIENTED_EDGE('',*,*,#1007,.F.);
#1410=ORIENTED_EDGE('',*,*,#914,.F.);
#1411=ORIENTED_EDGE('',*,*,#1006,.F.);
#1412=ORIENTED_EDGE('',*,*,#996,.F.);
#1413=ORIENTED_EDGE('',*,*,#1005,.F.);
#1414=ORIENTED_EDGE('',*,*,#1009,.T.);
#1415=ORIENTED_EDGE('',*,*,#1010,.T.);
#1416=ORIENTED_EDGE('',*,*,#1011,.T.);
#1417=ORIENTED_EDGE('',*,*,#1010,.F.);
#1418=ORIENTED_EDGE('',*,*,#1012,.F.);
#1419=ORIENTED_EDGE('',*,*,#1013,.T.);
#1420=ORIENTED_EDGE('',*,*,#1009,.F.);
#1421=ORIENTED_EDGE('',*,*,#1013,.F.);
#1422=ORIENTED_EDGE('',*,*,#1011,.F.);
#1423=ORIENTED_EDGE('',*,*,#1014,.T.);
#1424=ORIENTED_EDGE('',*,*,#1015,.T.);
#1425=ORIENTED_EDGE('',*,*,#1012,.T.);
#1426=ORIENTED_EDGE('',*,*,#1015,.F.);
#1427=ORIENTED_EDGE('',*,*,#1014,.F.);
#1428=ORIENTED_EDGE('',*,*,#1016,.T.);
#1429=ORIENTED_EDGE('',*,*,#1016,.F.);
#1430=ORIENTED_EDGE('',*,*,#1017,.F.);
#1431=ORIENTED_EDGE('',*,*,#1018,.F.);
#1432=ORIENTED_EDGE('',*,*,#1019,.T.);
#1433=ORIENTED_EDGE('',*,*,#1017,.T.);
#1434=ORIENTED_EDGE('',*,*,#1019,.F.);
#1435=ORIENTED_EDGE('',*,*,#1020,.F.);
#1436=ORIENTED_EDGE('',*,*,#1021,.T.);
#1437=ORIENTED_EDGE('',*,*,#1018,.T.);
#1438=ORIENTED_EDGE('',*,*,#1021,.F.);
#1439=ORIENTED_EDGE('',*,*,#1022,.F.);
#1440=ORIENTED_EDGE('',*,*,#1023,.T.);
#1441=ORIENTED_EDGE('',*,*,#1020,.T.);
#1442=ORIENTED_EDGE('',*,*,#1023,.F.);
#1443=ORIENTED_EDGE('',*,*,#1022,.T.);
#1444=CONICAL_SURFACE('',#1625,1.35,0.785398163397448);
#1445=CONICAL_SURFACE('',#1631,1.35,0.785398163397448);
#1446=CONICAL_SURFACE('',#1637,1.35,0.785398163397448);
#1447=CONICAL_SURFACE('',#1640,1.35,0.785398163397448);
#1448=CONICAL_SURFACE('',#1643,1.35,0.785398163397448);
#1449=CONICAL_SURFACE('',#1649,1.35,0.785398163397448);
#1450=CONICAL_SURFACE('',#1655,1.35,0.785398163397448);
#1451=CONICAL_SURFACE('',#1658,1.35,0.785398163397448);
#1452=CONICAL_SURFACE('',#1682,1.8,0.78539816339745);
#1453=CONICAL_SURFACE('',#1685,21.6,0.785398163397445);
#1454=CONICAL_SURFACE('',#1688,1.8,0.78539816339745);
#1455=CONICAL_SURFACE('',#1692,1.8,0.78539816339745);
#1456=CONICAL_SURFACE('',#1695,21.6,0.785398163397451);
#1457=CONICAL_SURFACE('',#1698,1.8,0.78539816339745);
#1458=CONICAL_SURFACE('',#1702,1.8,0.78539816339745);
#1459=CONICAL_SURFACE('',#1705,21.6,0.785398163397451);
#1460=CONICAL_SURFACE('',#1708,1.8,0.78539816339745);
#1461=CONICAL_SURFACE('',#1712,1.8,0.78539816339745);
#1462=CONICAL_SURFACE('',#1715,21.6,0.785398163397451);
#1463=CONICAL_SURFACE('',#1718,1.8,0.78539816339745);
#1464=CONICAL_SURFACE('',#1735,13.7,0.785398163397449);
#1465=CONICAL_SURFACE('',#1739,13.9,0.785398163397449);
#1466=CONICAL_SURFACE('',#1754,1.6,0.785398163397447);
#1467=CONICAL_SURFACE('',#1756,1.6,0.785398163397447);
#1468=CONICAL_SURFACE('',#1758,21.8,0.785398163397448);
#1469=CONICAL_SURFACE('',#1760,1.6,0.785398163397447);
#1470=CONICAL_SURFACE('',#1763,1.6,0.785398163397447);
#1471=CONICAL_SURFACE('',#1765,21.8,0.785398163397446);
#1472=CONICAL_SURFACE('',#1767,1.6,0.785398163397447);
#1473=CONICAL_SURFACE('',#1770,1.6,0.785398163397447);
#1474=CONICAL_SURFACE('',#1771,21.8,0.785398163397448);
#1475=CONICAL_SURFACE('',#1772,1.6,0.785398163397447);
#1476=CONICAL_SURFACE('',#1774,1.6,0.785398163397447);
#1477=CONICAL_SURFACE('',#1775,21.8,0.785398163397449);
#1478=CONICAL_SURFACE('',#1783,4.9,0.785398163397449);
#1479=CONICAL_SURFACE('',#1789,4.9,0.785398163397448);
#1480=CONICAL_SURFACE('',#1798,1.125,0.785398163397448);
#1481=CONICAL_SURFACE('',#1802,1.125,0.785398163397448);
#1482=ADVANCED_FACE('',(#191),#1444,.F.);
#1483=ADVANCED_FACE('',(#192,#139,#140),#169,.T.);
#1484=ADVANCED_FACE('',(#193),#108,.F.);
#1485=ADVANCED_FACE('',(#194),#1445,.F.);
#1486=ADVANCED_FACE('',(#195,#141,#142),#170,.T.);
#1487=ADVANCED_FACE('',(#196),#109,.F.);
#1488=ADVANCED_FACE('',(#197),#1446,.F.);
#1489=ADVANCED_FACE('',(#198),#110,.F.);
#1490=ADVANCED_FACE('',(#199),#1447,.F.);
#1491=ADVANCED_FACE('',(#200),#111,.F.);
#1492=ADVANCED_FACE('',(#201),#1448,.F.);
#1493=ADVANCED_FACE('',(#202,#143,#144),#171,.T.);
#1494=ADVANCED_FACE('',(#203),#112,.F.);
#1495=ADVANCED_FACE('',(#204),#1449,.F.);
#1496=ADVANCED_FACE('',(#205,#145,#146),#172,.T.);
#1497=ADVANCED_FACE('',(#206),#113,.F.);
#1498=ADVANCED_FACE('',(#207),#1450,.F.);
#1499=ADVANCED_FACE('',(#208),#114,.F.);
#1500=ADVANCED_FACE('',(#209),#1451,.F.);
#1501=ADVANCED_FACE('',(#210),#115,.F.);
#1502=ADVANCED_FACE('',(#211),#116,.F.);
#1503=ADVANCED_FACE('',(#212),#117,.F.);
#1504=ADVANCED_FACE('',(#213),#118,.F.);
#1505=ADVANCED_FACE('',(#214),#119,.F.);
#1506=ADVANCED_FACE('',(#215,#147,#148,#149,#150),#120,.F.);
#1507=ADVANCED_FACE('',(#216),#173,.T.);
#1508=ADVANCED_FACE('',(#217,#151,#152,#153,#154),#121,.F.);
#1509=ADVANCED_FACE('',(#218),#174,.T.);
#1510=ADVANCED_FACE('',(#219),#122,.F.);
#1511=ADVANCED_FACE('',(#220),#175,.T.);
#1512=ADVANCED_FACE('',(#221),#123,.F.);
#1513=ADVANCED_FACE('',(#222),#176,.T.);
#1514=ADVANCED_FACE('',(#223),#177,.T.);
#1515=ADVANCED_FACE('',(#224),#1452,.T.);
#1516=ADVANCED_FACE('',(#225),#1453,.F.);
#1517=ADVANCED_FACE('',(#226),#1454,.T.);
#1518=ADVANCED_FACE('',(#227),#178,.T.);
#1519=ADVANCED_FACE('',(#228),#1455,.T.);
#1520=ADVANCED_FACE('',(#229),#1456,.F.);
#1521=ADVANCED_FACE('',(#230),#1457,.T.);
#1522=ADVANCED_FACE('',(#231),#179,.T.);
#1523=ADVANCED_FACE('',(#232),#1458,.T.);
#1524=ADVANCED_FACE('',(#233),#1459,.F.);
#1525=ADVANCED_FACE('',(#234),#1460,.T.);
#1526=ADVANCED_FACE('',(#235),#180,.T.);
#1527=ADVANCED_FACE('',(#236),#1461,.T.);
#1528=ADVANCED_FACE('',(#237),#1462,.F.);
#1529=ADVANCED_FACE('',(#238),#1463,.T.);
#1530=ADVANCED_FACE('',(#239),#124,.T.);
#1531=ADVANCED_FACE('',(#240),#125,.F.);
#1532=ADVANCED_FACE('',(#241),#126,.T.);
#1533=ADVANCED_FACE('',(#242),#127,.T.);
#1534=ADVANCED_FACE('',(#243),#128,.F.);
#1535=ADVANCED_FACE('',(#244),#129,.T.);
#1536=ADVANCED_FACE('',(#245,#155),#181,.F.);
#1537=ADVANCED_FACE('',(#246),#1464,.F.);
#1538=ADVANCED_FACE('',(#247,#156,#157,#158,#159,#160,#161,#162,#163),#130,
 .F.);
#1539=ADVANCED_FACE('',(#248),#1465,.F.);
#1540=ADVANCED_FACE('',(#249,#164,#165,#166,#167,#168),#182,.T.);
#1541=ADVANCED_FACE('',(#250),#1466,.T.);
#1542=ADVANCED_FACE('',(#251),#183,.T.);
#1543=ADVANCED_FACE('',(#252),#1467,.T.);
#1544=ADVANCED_FACE('',(#253),#1468,.F.);
#1545=ADVANCED_FACE('',(#254),#1469,.T.);
#1546=ADVANCED_FACE('',(#255),#184,.T.);
#1547=ADVANCED_FACE('',(#256),#1470,.T.);
#1548=ADVANCED_FACE('',(#257),#1471,.F.);
#1549=ADVANCED_FACE('',(#258),#1472,.T.);
#1550=ADVANCED_FACE('',(#259),#185,.T.);
#1551=ADVANCED_FACE('',(#260),#1473,.T.);
#1552=ADVANCED_FACE('',(#261),#1474,.F.);
#1553=ADVANCED_FACE('',(#262),#1475,.T.);
#1554=ADVANCED_FACE('',(#263),#186,.T.);
#1555=ADVANCED_FACE('',(#264),#1476,.T.);
#1556=ADVANCED_FACE('',(#265),#1477,.F.);
#1557=ADVANCED_FACE('',(#266),#131,.T.);
#1558=ADVANCED_FACE('',(#267),#132,.T.);
#1559=ADVANCED_FACE('',(#268),#133,.T.);
#1560=ADVANCED_FACE('',(#269),#134,.T.);
#1561=ADVANCED_FACE('',(#270),#135,.F.);
#1562=ADVANCED_FACE('',(#271),#136,.F.);
#1563=ADVANCED_FACE('',(#272),#1478,.T.);
#1564=ADVANCED_FACE('',(#273),#137,.T.);
#1565=ADVANCED_FACE('',(#274),#187,.F.);
#1566=ADVANCED_FACE('',(#275),#1479,.T.);
#1567=ADVANCED_FACE('',(#276),#188,.T.);
#1568=ADVANCED_FACE('',(#277),#63,.T.);
#1569=ADVANCED_FACE('',(#278),#189,.T.);
#1570=ADVANCED_FACE('',(#279),#1480,.T.);
#1571=ADVANCED_FACE('',(#280),#138,.T.);
#1572=ADVANCED_FACE('',(#281),#1481,.T.);
#1573=ADVANCED_FACE('',(#282),#190,.T.);
#1574=CLOSED_SHELL('',(#1482,#1483,#1484,#1485,#1486,#1487,#1488,#1489,
#1490,#1491,#1492,#1493,#1494,#1495,#1496,#1497,#1498,#1499,#1500,#1501,
#1502,#1503,#1504,#1505,#1506,#1507,#1508,#1509,#1510,#1511,#1512,#1513,
#1514,#1515,#1516,#1517,#1518,#1519,#1520,#1521,#1522,#1523,#1524,#1525,
#1526,#1527,#1528,#1529,#1530,#1531,#1532,#1533,#1534,#1535,#1536,#1537,
#1538,#1539,#1540,#1541,#1542,#1543,#1544,#1545,#1546,#1547,#1548,#1549,
#1550,#1551,#1552,#1553,#1554,#1555,#1556,#1557,#1558,#1559,#1560,#1561,
#1562));
#1575=CLOSED_SHELL('',(#1563,#1564,#1565,#1566,#1567));
#1576=CLOSED_SHELL('',(#1568));
#1577=CLOSED_SHELL('',(#1569,#1570,#1571,#1572,#1573));
#1578=DERIVED_UNIT_ELEMENT(#1586,1.);
#1579=DERIVED_UNIT_ELEMENT(#3340,-3.);
#1580=DERIVED_UNIT_ELEMENT(#1586,1.);
#1581=DERIVED_UNIT_ELEMENT(#3340,-3.);
#1582=DERIVED_UNIT_ELEMENT(#1586,1.);
#1583=DERIVED_UNIT_ELEMENT(#3340,-3.);
#1584=DERIVED_UNIT_ELEMENT(#1586,1.);
#1585=DERIVED_UNIT_ELEMENT(#3340,-3.);
#1586=(
MASS_UNIT()
NAMED_UNIT(*)
SI_UNIT(.KILO.,.GRAM.)
);
#1587=DERIVED_UNIT((#1578,#1579));
#1588=DERIVED_UNIT((#1580,#1581));
#1589=DERIVED_UNIT((#1582,#1583));
#1590=DERIVED_UNIT((#1584,#1585));
#1591=MEASURE_REPRESENTATION_ITEM('density measure',
POSITIVE_RATIO_MEASURE(7850.),#1587);
#1592=MEASURE_REPRESENTATION_ITEM('density measure',
POSITIVE_RATIO_MEASURE(7850.),#1588);
#1593=MEASURE_REPRESENTATION_ITEM('density measure',
POSITIVE_RATIO_MEASURE(7850.),#1589);
#1594=MEASURE_REPRESENTATION_ITEM('density measure',
POSITIVE_RATIO_MEASURE(7850.),#1590);
#1595=PROPERTY_DEFINITION_REPRESENTATION(#1615,#1603);
#1596=PROPERTY_DEFINITION_REPRESENTATION(#1616,#1604);
#1597=PROPERTY_DEFINITION_REPRESENTATION(#1617,#1605);
#1598=PROPERTY_DEFINITION_REPRESENTATION(#1618,#1606);
#1599=PROPERTY_DEFINITION_REPRESENTATION(#1619,#1607);
#1600=PROPERTY_DEFINITION_REPRESENTATION(#1620,#1608);
#1601=PROPERTY_DEFINITION_REPRESENTATION(#1621,#1609);
#1602=PROPERTY_DEFINITION_REPRESENTATION(#1622,#1610);
#1603=REPRESENTATION('material name',(#1611),#3334);
#1604=REPRESENTATION('density',(#1591),#3334);
#1605=REPRESENTATION('material name',(#1612),#3335);
#1606=REPRESENTATION('density',(#1592),#3335);
#1607=REPRESENTATION('material name',(#1613),#3336);
#1608=REPRESENTATION('density',(#1593),#3336);
#1609=REPRESENTATION('material name',(#1614),#3337);
#1610=REPRESENTATION('density',(#1594),#3337);
#1611=DESCRIPTIVE_REPRESENTATION_ITEM('Steel','Steel');
#1612=DESCRIPTIVE_REPRESENTATION_ITEM('Steel','Steel');
#1613=DESCRIPTIVE_REPRESENTATION_ITEM('Steel','Steel');
#1614=DESCRIPTIVE_REPRESENTATION_ITEM('Steel','Steel');
#1615=PROPERTY_DEFINITION('material property','material name',#3373);
#1616=PROPERTY_DEFINITION('material property','density of part',#3373);
#1617=PROPERTY_DEFINITION('material property','material name',#3374);
#1618=PROPERTY_DEFINITION('material property','density of part',#3374);
#1619=PROPERTY_DEFINITION('material property','material name',#3375);
#1620=PROPERTY_DEFINITION('material property','density of part',#3375);
#1621=PROPERTY_DEFINITION('material property','material name',#3376);
#1622=PROPERTY_DEFINITION('material property','density of part',#3376);
#1623=AXIS2_PLACEMENT_3D('',#2305,#1818,#1819);
#1624=AXIS2_PLACEMENT_3D('',#2306,#1820,#1821);
#1625=AXIS2_PLACEMENT_3D('',#2307,#1822,#1823);
#1626=AXIS2_PLACEMENT_3D('',#2309,#1824,#1825);
#1627=AXIS2_PLACEMENT_3D('',#2312,#1827,#1828);
#1628=AXIS2_PLACEMENT_3D('',#2313,#1829,#1830);
#1629=AXIS2_PLACEMENT_3D('',#2323,#1835,#1836);
#1630=AXIS2_PLACEMENT_3D('',#2324,#1837,#1838);
#1631=AXIS2_PLACEMENT_3D('',#2368,#1840,#1841);
#1632=AXIS2_PLACEMENT_3D('',#2370,#1842,#1843);
#1633=AXIS2_PLACEMENT_3D('',#2373,#1845,#1846);
#1634=AXIS2_PLACEMENT_3D('',#2374,#1847,#1848);
#1635=AXIS2_PLACEMENT_3D('',#2384,#1853,#1854);
#1636=AXIS2_PLACEMENT_3D('',#2385,#1855,#1856);
#1637=AXIS2_PLACEMENT_3D('',#2429,#1858,#1859);
#1638=AXIS2_PLACEMENT_3D('',#2432,#1861,#1862);
#1639=AXIS2_PLACEMENT_3D('',#2433,#1863,#1864);
#1640=AXIS2_PLACEMENT_3D('',#2477,#1866,#1867);
#1641=AXIS2_PLACEMENT_3D('',#2480,#1869,#1870);
#1642=AXIS2_PLACEMENT_3D('',#2481,#1871,#1872);
#1643=AXIS2_PLACEMENT_3D('',#2525,#1874,#1875);
#1644=AXIS2_PLACEMENT_3D('',#2527,#1876,#1877);
#1645=AXIS2_PLACEMENT_3D('',#2530,#1879,#1880);
#1646=AXIS2_PLACEMENT_3D('',#2531,#1881,#1882);
#1647=AXIS2_PLACEMENT_3D('',#2541,#1887,#1888);
#1648=AXIS2_PLACEMENT_3D('',#2542,#1889,#1890);
#1649=AXIS2_PLACEMENT_3D('',#2579,#1892,#1893);
#1650=AXIS2_PLACEMENT_3D('',#2581,#1894,#1895);
#1651=AXIS2_PLACEMENT_3D('',#2584,#1897,#1898);
#1652=AXIS2_PLACEMENT_3D('',#2585,#1899,#1900);
#1653=AXIS2_PLACEMENT_3D('',#2595,#1905,#1906);
#1654=AXIS2_PLACEMENT_3D('',#2596,#1907,#1908);
#1655=AXIS2_PLACEMENT_3D('',#2633,#1910,#1911);
#1656=AXIS2_PLACEMENT_3D('',#2636,#1913,#1914);
#1657=AXIS2_PLACEMENT_3D('',#2637,#1915,#1916);
#1658=AXIS2_PLACEMENT_3D('',#2674,#1918,#1919);
#1659=AXIS2_PLACEMENT_3D('',#2677,#1921,#1922);
#1660=AXIS2_PLACEMENT_3D('',#2678,#1923,#1924);
#1661=AXIS2_PLACEMENT_3D('',#2715,#1926,#1927);
#1662=AXIS2_PLACEMENT_3D('',#2797,#1929,#1930);
#1663=AXIS2_PLACEMENT_3D('',#2879,#1932,#1933);
#1664=AXIS2_PLACEMENT_3D('',#2961,#1935,#1936);
#1665=AXIS2_PLACEMENT_3D('',#3043,#1938,#1939);
#1666=AXIS2_PLACEMENT_3D('',#3045,#1940,#1941);
#1667=AXIS2_PLACEMENT_3D('',#3048,#1943,#1944);
#1668=AXIS2_PLACEMENT_3D('',#3049,#1945,#1946);
#1669=AXIS2_PLACEMENT_3D('',#3050,#1947,#1948);
#1670=AXIS2_PLACEMENT_3D('',#3052,#1949,#1950);
#1671=AXIS2_PLACEMENT_3D('',#3055,#1952,#1953);
#1672=AXIS2_PLACEMENT_3D('',#3056,#1954,#1955);
#1673=AXIS2_PLACEMENT_3D('',#3057,#1956,#1957);
#1674=AXIS2_PLACEMENT_3D('',#3059,#1958,#1959);
#1675=AXIS2_PLACEMENT_3D('',#3062,#1961,#1962);
#1676=AXIS2_PLACEMENT_3D('',#3063,#1963,#1964);
#1677=AXIS2_PLACEMENT_3D('',#3064,#1965,#1966);
#1678=AXIS2_PLACEMENT_3D('',#3066,#1967,#1968);
#1679=AXIS2_PLACEMENT_3D('',#3069,#1970,#1971);
#1680=AXIS2_PLACEMENT_3D('',#3070,#1972,#1973);
#1681=AXIS2_PLACEMENT_3D('',#3071,#1974,#1975);
#1682=AXIS2_PLACEMENT_3D('',#3077,#1979,#1980);
#1683=AXIS2_PLACEMENT_3D('',#3081,#1982,#1983);
#1684=AXIS2_PLACEMENT_3D('',#3082,#1984,#1985);
#1685=AXIS2_PLACEMENT_3D('',#3083,#1986,#1987);
#1686=AXIS2_PLACEMENT_3D('',#3085,#1988,#1989);
#1687=AXIS2_PLACEMENT_3D('',#3088,#1991,#1992);
#1688=AXIS2_PLACEMENT_3D('',#3089,#1993,#1994);
#1689=AXIS2_PLACEMENT_3D('',#3092,#1996,#1997);
#1690=AXIS2_PLACEMENT_3D('',#3093,#1998,#1999);
#1691=AXIS2_PLACEMENT_3D('',#3094,#2000,#2001);
#1692=AXIS2_PLACEMENT_3D('',#3098,#2004,#2005);
#1693=AXIS2_PLACEMENT_3D('',#3102,#2007,#2008);
#1694=AXIS2_PLACEMENT_3D('',#3103,#2009,#2010);
#1695=AXIS2_PLACEMENT_3D('',#3104,#2011,#2012);
#1696=AXIS2_PLACEMENT_3D('',#3106,#2013,#2014);
#1697=AXIS2_PLACEMENT_3D('',#3109,#2016,#2017);
#1698=AXIS2_PLACEMENT_3D('',#3110,#2018,#2019);
#1699=AXIS2_PLACEMENT_3D('',#3113,#2021,#2022);
#1700=AXIS2_PLACEMENT_3D('',#3114,#2023,#2024);
#1701=AXIS2_PLACEMENT_3D('',#3115,#2025,#2026);
#1702=AXIS2_PLACEMENT_3D('',#3119,#2029,#2030);
#1703=AXIS2_PLACEMENT_3D('',#3123,#2032,#2033);
#1704=AXIS2_PLACEMENT_3D('',#3124,#2034,#2035);
#1705=AXIS2_PLACEMENT_3D('',#3125,#2036,#2037);
#1706=AXIS2_PLACEMENT_3D('',#3127,#2038,#2039);
#1707=AXIS2_PLACEMENT_3D('',#3130,#2041,#2042);
#1708=AXIS2_PLACEMENT_3D('',#3131,#2043,#2044);
#1709=AXIS2_PLACEMENT_3D('',#3134,#2046,#2047);
#1710=AXIS2_PLACEMENT_3D('',#3135,#2048,#2049);
#1711=AXIS2_PLACEMENT_3D('',#3136,#2050,#2051);
#1712=AXIS2_PLACEMENT_3D('',#3140,#2054,#2055);
#1713=AXIS2_PLACEMENT_3D('',#3144,#2057,#2058);
#1714=AXIS2_PLACEMENT_3D('',#3145,#2059,#2060);
#1715=AXIS2_PLACEMENT_3D('',#3146,#2061,#2062);
#1716=AXIS2_PLACEMENT_3D('',#3148,#2063,#2064);
#1717=AXIS2_PLACEMENT_3D('',#3151,#2066,#2067);
#1718=AXIS2_PLACEMENT_3D('',#3152,#2068,#2069);
#1719=AXIS2_PLACEMENT_3D('',#3153,#2070,#2071);
#1720=AXIS2_PLACEMENT_3D('',#3154,#2072,#2073);
#1721=AXIS2_PLACEMENT_3D('',#3155,#2074,#2075);
#1722=AXIS2_PLACEMENT_3D('',#3158,#2077,#2078);
#1723=AXIS2_PLACEMENT_3D('',#3159,#2079,#2080);
#1724=AXIS2_PLACEMENT_3D('',#3162,#2082,#2083);
#1725=AXIS2_PLACEMENT_3D('',#3163,#2084,#2085);
#1726=AXIS2_PLACEMENT_3D('',#3164,#2086,#2087);
#1727=AXIS2_PLACEMENT_3D('',#3165,#2088,#2089);
#1728=AXIS2_PLACEMENT_3D('',#3168,#2091,#2092);
#1729=AXIS2_PLACEMENT_3D('',#3169,#2093,#2094);
#1730=AXIS2_PLACEMENT_3D('',#3172,#2096,#2097);
#1731=AXIS2_PLACEMENT_3D('',#3173,#2098,#2099);
#1732=AXIS2_PLACEMENT_3D('',#3174,#2100,#2101);
#1733=AXIS2_PLACEMENT_3D('',#3175,#2102,#2103);
#1734=AXIS2_PLACEMENT_3D('',#3177,#2104,#2105);
#1735=AXIS2_PLACEMENT_3D('',#3178,#2106,#2107);
#1736=AXIS2_PLACEMENT_3D('',#3180,#2108,#2109);
#1737=AXIS2_PLACEMENT_3D('',#3182,#2111,#2112);
#1738=AXIS2_PLACEMENT_3D('',#3184,#2113,#2114);
#1739=AXIS2_PLACEMENT_3D('',#3186,#2116,#2117);
#1740=AXIS2_PLACEMENT_3D('',#3188,#2118,#2119);
#1741=AXIS2_PLACEMENT_3D('',#3190,#2121,#2122);
#1742=AXIS2_PLACEMENT_3D('',#3193,#2123,#2124);
#1743=AXIS2_PLACEMENT_3D('',#3195,#2125,#2126);
#1744=AXIS2_PLACEMENT_3D('',#3197,#2127,#2128);
#1745=AXIS2_PLACEMENT_3D('',#3201,#2130,#2131);
#1746=AXIS2_PLACEMENT_3D('',#3203,#2132,#2133);
#1747=AXIS2_PLACEMENT_3D('',#3205,#2134,#2135);
#1748=AXIS2_PLACEMENT_3D('',#3209,#2137,#2138);
#1749=AXIS2_PLACEMENT_3D('',#3211,#2139,#2140);
#1750=AXIS2_PLACEMENT_3D('',#3213,#2141,#2142);
#1751=AXIS2_PLACEMENT_3D('',#3217,#2144,#2145);
#1752=AXIS2_PLACEMENT_3D('',#3219,#2146,#2147);
#1753=AXIS2_PLACEMENT_3D('',#3221,#2148,#2149);
#1754=AXIS2_PLACEMENT_3D('',#3223,#2151,#2152);
#1755=AXIS2_PLACEMENT_3D('',#3226,#2155,#2156);
#1756=AXIS2_PLACEMENT_3D('',#3228,#2158,#2159);
#1757=AXIS2_PLACEMENT_3D('',#3231,#2161,#2162);
#1758=AXIS2_PLACEMENT_3D('',#3232,#2163,#2164);
#1759=AXIS2_PLACEMENT_3D('',#3235,#2166,#2167);
#1760=AXIS2_PLACEMENT_3D('',#3236,#2168,#2169);
#1761=AXIS2_PLACEMENT_3D('',#3238,#2171,#2172);
#1762=AXIS2_PLACEMENT_3D('',#3239,#2173,#2174);
#1763=AXIS2_PLACEMENT_3D('',#3241,#2176,#2177);
#1764=AXIS2_PLACEMENT_3D('',#3244,#2179,#2180);
#1765=AXIS2_PLACEMENT_3D('',#3245,#2181,#2182);
#1766=AXIS2_PLACEMENT_3D('',#3248,#2184,#2185);
#1767=AXIS2_PLACEMENT_3D('',#3249,#2186,#2187);
#1768=AXIS2_PLACEMENT_3D('',#3251,#2189,#2190);
#1769=AXIS2_PLACEMENT_3D('',#3252,#2191,#2192);
#1770=AXIS2_PLACEMENT_3D('',#3254,#2194,#2195);
#1771=AXIS2_PLACEMENT_3D('',#3256,#2197,#2198);
#1772=AXIS2_PLACEMENT_3D('',#3258,#2200,#2201);
#1773=AXIS2_PLACEMENT_3D('',#3260,#2203,#2204);
#1774=AXIS2_PLACEMENT_3D('',#3262,#2206,#2207);
#1775=AXIS2_PLACEMENT_3D('',#3264,#2209,#2210);
#1776=AXIS2_PLACEMENT_3D('',#3265,#2211,#2212);
#1777=AXIS2_PLACEMENT_3D('',#3267,#2214,#2215);
#1778=AXIS2_PLACEMENT_3D('',#3269,#2217,#2218);
#1779=AXIS2_PLACEMENT_3D('',#3271,#2220,#2221);
#1780=AXIS2_PLACEMENT_3D('',#3273,#2223,#2224);
#1781=AXIS2_PLACEMENT_3D('',#3274,#2225,#2226);
#1782=AXIS2_PLACEMENT_3D('',#3275,#2227,#2228);
#1783=AXIS2_PLACEMENT_3D('',#3276,#2229,#2230);
#1784=AXIS2_PLACEMENT_3D('',#3278,#2231,#2232);
#1785=AXIS2_PLACEMENT_3D('',#3281,#2234,#2235);
#1786=AXIS2_PLACEMENT_3D('',#3282,#2236,#2237);
#1787=AXIS2_PLACEMENT_3D('',#3284,#2238,#2239);
#1788=AXIS2_PLACEMENT_3D('',#3286,#2241,#2242);
#1789=AXIS2_PLACEMENT_3D('',#3287,#2243,#2244);
#1790=AXIS2_PLACEMENT_3D('',#3289,#2245,#2246);
#1791=AXIS2_PLACEMENT_3D('',#3291,#2248,#2249);
#1792=AXIS2_PLACEMENT_3D('',#3292,#2250,#2251);
#1793=AXIS2_PLACEMENT_3D('',#3293,#2252,#2253);
#1794=AXIS2_PLACEMENT_3D('',#3296,#2254,#2255);
#1795=AXIS2_PLACEMENT_3D('',#3297,#2256,#2257);
#1796=AXIS2_PLACEMENT_3D('',#3298,#2258,#2259);
#1797=AXIS2_PLACEMENT_3D('',#3300,#2260,#2261);
#1798=AXIS2_PLACEMENT_3D('',#3301,#2262,#2263);
#1799=AXIS2_PLACEMENT_3D('',#3303,#2264,#2265);
#1800=AXIS2_PLACEMENT_3D('',#3305,#2267,#2268);
#1801=AXIS2_PLACEMENT_3D('',#3307,#2269,#2270);
#1802=AXIS2_PLACEMENT_3D('',#3309,#2272,#2273);
#1803=AXIS2_PLACEMENT_3D('',#3311,#2274,#2275);
#1804=AXIS2_PLACEMENT_3D('',#3313,#2277,#2278);
#1805=AXIS2_PLACEMENT_3D('',#3314,#2279,#2280);
#1806=AXIS2_PLACEMENT_3D('',#3315,#2281,#2282);
#1807=AXIS2_PLACEMENT_3D('',#3316,#2283,#2284);
#1808=AXIS2_PLACEMENT_3D('',#3317,#2285,#2286);
#1809=AXIS2_PLACEMENT_3D('',#3318,#2287,#2288);
#1810=AXIS2_PLACEMENT_3D('',#3319,#2289,#2290);
#1811=AXIS2_PLACEMENT_3D('',#3320,#2291,#2292);
#1812=AXIS2_PLACEMENT_3D('',#3321,#2293,#2294);
#1813=AXIS2_PLACEMENT_3D('',#3322,#2295,#2296);
#1814=AXIS2_PLACEMENT_3D('',#3323,#2297,#2298);
#1815=AXIS2_PLACEMENT_3D('',#3324,#2299,#2300);
#1816=AXIS2_PLACEMENT_3D('',#3325,#2301,#2302);
#1817=AXIS2_PLACEMENT_3D('',#3326,#2303,#2304);
#1818=DIRECTION('axis',(0.,0.,1.));
#1819=DIRECTION('refdir',(1.,0.,0.));
#1820=DIRECTION('axis',(0.,0.,1.));
#1821=DIRECTION('refdir',(1.,0.,0.));
#1822=DIRECTION('center_axis',(1.,0.,0.));
#1823=DIRECTION('ref_axis',(0.,0.,-1.));
#1824=DIRECTION('center_axis',(1.,0.,0.));
#1825=DIRECTION('ref_axis',(0.,0.,-1.));
#1826=DIRECTION('',(-0.707106781186548,8.65956056235493E-17,-0.707106781186548));
#1827=DIRECTION('center_axis',(-1.,0.,0.));
#1828=DIRECTION('ref_axis',(0.,0.,-1.));
#1829=DIRECTION('center_axis',(1.,0.,0.));
#1830=DIRECTION('ref_axis',(0.,1.,0.));
#1831=DIRECTION('',(0.,-1.,0.));
#1832=DIRECTION('',(0.,0.,-1.));
#1833=DIRECTION('',(0.,1.,0.));
#1834=DIRECTION('',(0.,0.,1.));
#1835=DIRECTION('center_axis',(1.,0.,0.));
#1836=DIRECTION('ref_axis',(0.,0.,-1.));
#1837=DIRECTION('center_axis',(1.,0.,0.));
#1838=DIRECTION('ref_axis',(0.,0.,-1.));
#1839=DIRECTION('',(1.,0.,0.));
#1840=DIRECTION('center_axis',(-1.,0.,0.));
#1841=DIRECTION('ref_axis',(0.,0.,-1.));
#1842=DIRECTION('center_axis',(-1.,0.,0.));
#1843=DIRECTION('ref_axis',(0.,0.,-1.));
#1844=DIRECTION('',(0.707106781186548,-8.65956056235493E-17,-0.707106781186548));
#1845=DIRECTION('center_axis',(1.,0.,0.));
#1846=DIRECTION('ref_axis',(0.,0.,-1.));
#1847=DIRECTION('center_axis',(-1.,0.,0.));
#1848=DIRECTION('ref_axis',(0.,-1.,0.));
#1849=DIRECTION('',(0.,1.,0.));
#1850=DIRECTION('',(0.,0.,-1.));
#1851=DIRECTION('',(0.,-1.,0.));
#1852=DIRECTION('',(0.,0.,1.));
#1853=DIRECTION('center_axis',(-1.,0.,0.));
#1854=DIRECTION('ref_axis',(0.,0.,-1.));
#1855=DIRECTION('center_axis',(1.,0.,0.));
#1856=DIRECTION('ref_axis',(0.,0.,-1.));
#1857=DIRECTION('',(1.,0.,0.));
#1858=DIRECTION('center_axis',(1.,0.,0.));
#1859=DIRECTION('ref_axis',(0.,0.,-1.));
#1860=DIRECTION('',(-0.707106781186548,8.65956056235493E-17,-0.707106781186548));
#1861=DIRECTION('center_axis',(-1.,0.,0.));
#1862=DIRECTION('ref_axis',(0.,0.,-1.));
#1863=DIRECTION('center_axis',(1.,0.,0.));
#1864=DIRECTION('ref_axis',(0.,0.,-1.));
#1865=DIRECTION('',(1.,0.,0.));
#1866=DIRECTION('center_axis',(-1.,0.,0.));
#1867=DIRECTION('ref_axis',(0.,0.,-1.));
#1868=DIRECTION('',(0.707106781186548,-8.65956056235493E-17,-0.707106781186548));
#1869=DIRECTION('center_axis',(1.,0.,0.));
#1870=DIRECTION('ref_axis',(0.,0.,-1.));
#1871=DIRECTION('center_axis',(1.,0.,0.));
#1872=DIRECTION('ref_axis',(0.,0.,-1.));
#1873=DIRECTION('',(1.,0.,0.));
#1874=DIRECTION('center_axis',(0.,1.,0.));
#1875=DIRECTION('ref_axis',(1.,0.,0.));
#1876=DIRECTION('center_axis',(0.,1.,0.));
#1877=DIRECTION('ref_axis',(1.,0.,0.));
#1878=DIRECTION('',(0.707106781186548,-0.707106781186548,-8.65956056235493E-17));
#1879=DIRECTION('center_axis',(0.,-1.,0.));
#1880=DIRECTION('ref_axis',(1.,0.,0.));
#1881=DIRECTION('center_axis',(0.,1.,0.));
#1882=DIRECTION('ref_axis',(-1.,0.,0.));
#1883=DIRECTION('',(1.,0.,0.));
#1884=DIRECTION('',(0.,0.,-1.));
#1885=DIRECTION('',(-1.,0.,0.));
#1886=DIRECTION('',(0.,0.,1.));
#1887=DIRECTION('center_axis',(0.,1.,0.));
#1888=DIRECTION('ref_axis',(1.,0.,0.));
#1889=DIRECTION('center_axis',(0.,1.,0.));
#1890=DIRECTION('ref_axis',(1.,0.,0.));
#1891=DIRECTION('',(0.,1.,0.));
#1892=DIRECTION('center_axis',(0.,-1.,0.));
#1893=DIRECTION('ref_axis',(1.,0.,0.));
#1894=DIRECTION('center_axis',(0.,-1.,0.));
#1895=DIRECTION('ref_axis',(1.,0.,0.));
#1896=DIRECTION('',(0.707106781186548,0.707106781186548,8.65956056235493E-17));
#1897=DIRECTION('center_axis',(0.,1.,0.));
#1898=DIRECTION('ref_axis',(1.,0.,0.));
#1899=DIRECTION('center_axis',(0.,-1.,0.));
#1900=DIRECTION('ref_axis',(1.,0.,0.));
#1901=DIRECTION('',(-1.,0.,0.));
#1902=DIRECTION('',(0.,0.,-1.));
#1903=DIRECTION('',(1.,0.,0.));
#1904=DIRECTION('',(0.,0.,1.));
#1905=DIRECTION('center_axis',(0.,-1.,0.));
#1906=DIRECTION('ref_axis',(1.,0.,0.));
#1907=DIRECTION('center_axis',(0.,1.,0.));
#1908=DIRECTION('ref_axis',(1.,0.,0.));
#1909=DIRECTION('',(0.,1.,0.));
#1910=DIRECTION('center_axis',(0.,1.,0.));
#1911=DIRECTION('ref_axis',(1.,0.,0.));
#1912=DIRECTION('',(0.707106781186548,-0.707106781186548,-8.65956056235493E-17));
#1913=DIRECTION('center_axis',(0.,-1.,0.));
#1914=DIRECTION('ref_axis',(1.,0.,0.));
#1915=DIRECTION('center_axis',(0.,1.,0.));
#1916=DIRECTION('ref_axis',(1.,0.,0.));
#1917=DIRECTION('',(0.,1.,0.));
#1918=DIRECTION('center_axis',(0.,-1.,0.));
#1919=DIRECTION('ref_axis',(1.,0.,0.));
#1920=DIRECTION('',(0.707106781186548,0.707106781186548,8.65956056235493E-17));
#1921=DIRECTION('center_axis',(0.,1.,0.));
#1922=DIRECTION('ref_axis',(1.,0.,0.));
#1923=DIRECTION('center_axis',(0.,1.,0.));
#1924=DIRECTION('ref_axis',(1.,0.,0.));
#1925=DIRECTION('',(0.,1.,0.));
#1926=DIRECTION('center_axis',(1.,0.,0.));
#1927=DIRECTION('ref_axis',(0.,0.,-1.));
#1928=DIRECTION('',(1.,0.,0.));
#1929=DIRECTION('center_axis',(1.,0.,0.));
#1930=DIRECTION('ref_axis',(0.,0.,-1.));
#1931=DIRECTION('',(1.,0.,0.));
#1932=DIRECTION('center_axis',(1.,0.,0.));
#1933=DIRECTION('ref_axis',(0.,0.,-1.));
#1934=DIRECTION('',(1.,0.,0.));
#1935=DIRECTION('center_axis',(1.,0.,0.));
#1936=DIRECTION('ref_axis',(0.,0.,-1.));
#1937=DIRECTION('',(1.,0.,0.));
#1938=DIRECTION('center_axis',(0.,0.,1.));
#1939=DIRECTION('ref_axis',(0.,1.,0.));
#1940=DIRECTION('center_axis',(0.,0.,1.));
#1941=DIRECTION('ref_axis',(0.,1.,0.));
#1942=DIRECTION('',(0.,0.,1.));
#1943=DIRECTION('center_axis',(0.,0.,-1.));
#1944=DIRECTION('ref_axis',(0.,1.,0.));
#1945=DIRECTION('center_axis',(0.,0.,1.));
#1946=DIRECTION('ref_axis',(1.,0.,0.));
#1947=DIRECTION('center_axis',(0.,0.,1.));
#1948=DIRECTION('ref_axis',(0.,1.,0.));
#1949=DIRECTION('center_axis',(0.,0.,1.));
#1950=DIRECTION('ref_axis',(0.,1.,0.));
#1951=DIRECTION('',(0.,0.,1.));
#1952=DIRECTION('center_axis',(0.,0.,-1.));
#1953=DIRECTION('ref_axis',(0.,1.,0.));
#1954=DIRECTION('center_axis',(0.,0.,1.));
#1955=DIRECTION('ref_axis',(1.,0.,0.));
#1956=DIRECTION('center_axis',(0.,0.,1.));
#1957=DIRECTION('ref_axis',(1.,0.,0.));
#1958=DIRECTION('center_axis',(0.,0.,1.));
#1959=DIRECTION('ref_axis',(1.,0.,0.));
#1960=DIRECTION('',(0.,0.,1.));
#1961=DIRECTION('center_axis',(0.,0.,-1.));
#1962=DIRECTION('ref_axis',(1.,0.,0.));
#1963=DIRECTION('center_axis',(0.,0.,1.));
#1964=DIRECTION('ref_axis',(1.,0.,0.));
#1965=DIRECTION('center_axis',(0.,0.,1.));
#1966=DIRECTION('ref_axis',(1.,0.,0.));
#1967=DIRECTION('center_axis',(0.,0.,1.));
#1968=DIRECTION('ref_axis',(1.,0.,0.));
#1969=DIRECTION('',(0.,0.,1.));
#1970=DIRECTION('center_axis',(0.,0.,-1.));
#1971=DIRECTION('ref_axis',(1.,0.,0.));
#1972=DIRECTION('center_axis',(0.,0.,1.));
#1973=DIRECTION('ref_axis',(1.,0.,0.));
#1974=DIRECTION('center_axis',(0.,-0.707106781186547,-0.707106781186548));
#1975=DIRECTION('ref_axis',(-1.,0.,0.));
#1976=DIRECTION('',(-1.96261557335472E-15,-0.707106781186548,0.707106781186547));
#1977=DIRECTION('',(0.,0.707106781186548,-0.707106781186547));
#1978=DIRECTION('',(1.,0.,0.));
#1979=DIRECTION('center_axis',(0.,0.,1.));
#1980=DIRECTION('ref_axis',(0.639511031159242,-0.768781920329584,0.));
#1981=DIRECTION('',(0.695290346079778,-0.128729696062163,0.707106781186551));
#1982=DIRECTION('center_axis',(0.,0.,-1.));
#1983=DIRECTION('ref_axis',(0.639511031159242,-0.768781920329584,0.));
#1984=DIRECTION('center_axis',(0.,0.,1.));
#1985=DIRECTION('ref_axis',(0.639511031159242,-0.768781920329584,0.));
#1986=DIRECTION('center_axis',(0.,0.,-1.));
#1987=DIRECTION('ref_axis',(-0.105607476635515,0.994407894618038,0.));
#1988=DIRECTION('center_axis',(0.,0.,-1.));
#1989=DIRECTION('ref_axis',(-0.105607476635515,0.994407894618038,0.));
#1990=DIRECTION('',(0.128729696062162,-0.695290346079783,0.707106781186546));
#1991=DIRECTION('center_axis',(0.,0.,1.));
#1992=DIRECTION('ref_axis',(-0.105607476635515,0.994407894618038,0.));
#1993=DIRECTION('center_axis',(0.,0.,1.));
#1994=DIRECTION('ref_axis',(0.768781920329583,-0.639511031159243,0.));
#1995=DIRECTION('',(0.707106781186548,0.,0.707106781186547));
#1996=DIRECTION('center_axis',(0.,0.,-1.));
#1997=DIRECTION('ref_axis',(0.768781920329583,-0.639511031159243,0.));
#1998=DIRECTION('center_axis',(0.,0.,1.));
#1999=DIRECTION('ref_axis',(0.768781920329583,-0.639511031159243,0.));
#2000=DIRECTION('center_axis',(0.707106781186547,0.,-0.707106781186548));
#2001=DIRECTION('ref_axis',(-0.707106781186548,0.,-0.707106781186547));
#2002=DIRECTION('',(0.707106781186548,0.,0.707106781186547));
#2003=DIRECTION('',(0.,1.,0.));
#2004=DIRECTION('center_axis',(0.,0.,1.));
#2005=DIRECTION('ref_axis',(0.768781920329583,0.639511031159243,0.));
#2006=DIRECTION('',(0.12872969606217,0.695290346079785,0.707106781186544));
#2007=DIRECTION('center_axis',(0.,0.,-1.));
#2008=DIRECTION('ref_axis',(0.768781920329583,0.639511031159243,0.));
#2009=DIRECTION('center_axis',(0.,0.,1.));
#2010=DIRECTION('ref_axis',(0.768781920329583,0.639511031159243,0.));
#2011=DIRECTION('center_axis',(0.,0.,-1.));
#2012=DIRECTION('ref_axis',(-0.994407894618038,-0.105607476635514,0.));
#2013=DIRECTION('center_axis',(0.,0.,-1.));
#2014=DIRECTION('ref_axis',(-0.994407894618038,-0.105607476635514,0.));
#2015=DIRECTION('',(0.695290346079784,0.12872969606217,0.707106781186545));
#2016=DIRECTION('center_axis',(0.,0.,1.));
#2017=DIRECTION('ref_axis',(-0.994407894618038,-0.105607476635514,0.));
#2018=DIRECTION('center_axis',(0.,0.,1.));
#2019=DIRECTION('ref_axis',(0.639511031159243,0.768781920329583,0.));
#2020=DIRECTION('',(0.,0.707106781186548,0.707106781186547));
#2021=DIRECTION('center_axis',(0.,0.,-1.));
#2022=DIRECTION('ref_axis',(0.639511031159243,0.768781920329583,0.));
#2023=DIRECTION('center_axis',(0.,0.,1.));
#2024=DIRECTION('ref_axis',(0.639511031159243,0.768781920329583,0.));
#2025=DIRECTION('center_axis',(0.,0.707106781186547,-0.707106781186548));
#2026=DIRECTION('ref_axis',(-1.,0.,0.));
#2027=DIRECTION('',(0.,0.707106781186548,0.707106781186547));
#2028=DIRECTION('',(-1.,0.,0.));
#2029=DIRECTION('center_axis',(0.,0.,1.));
#2030=DIRECTION('ref_axis',(-0.639511031159243,0.768781920329583,0.));
#2031=DIRECTION('',(-0.695290346079785,0.12872969606217,0.707106781186544));
#2032=DIRECTION('center_axis',(0.,0.,-1.));
#2033=DIRECTION('ref_axis',(-0.639511031159243,0.768781920329583,0.));
#2034=DIRECTION('center_axis',(0.,0.,1.));
#2035=DIRECTION('ref_axis',(-0.639511031159243,0.768781920329583,0.));
#2036=DIRECTION('center_axis',(0.,0.,-1.));
#2037=DIRECTION('ref_axis',(0.105607476635514,-0.994407894618038,0.));
#2038=DIRECTION('center_axis',(0.,0.,-1.));
#2039=DIRECTION('ref_axis',(0.105607476635514,-0.994407894618038,0.));
#2040=DIRECTION('',(-0.12872969606217,0.695290346079784,0.707106781186545));
#2041=DIRECTION('center_axis',(0.,0.,1.));
#2042=DIRECTION('ref_axis',(0.105607476635514,-0.994407894618038,0.));
#2043=DIRECTION('center_axis',(0.,0.,1.));
#2044=DIRECTION('ref_axis',(-0.768781920329583,0.639511031159243,0.));
#2045=DIRECTION('',(-0.707106781186548,0.,0.707106781186547));
#2046=DIRECTION('center_axis',(0.,0.,-1.));
#2047=DIRECTION('ref_axis',(-0.768781920329583,0.639511031159243,0.));
#2048=DIRECTION('center_axis',(0.,0.,1.));
#2049=DIRECTION('ref_axis',(-0.768781920329583,0.639511031159243,0.));
#2050=DIRECTION('center_axis',(-0.707106781186547,0.,-0.707106781186548));
#2051=DIRECTION('ref_axis',(-0.707106781186548,0.,0.707106781186547));
#2052=DIRECTION('',(-0.707106781186548,0.,0.707106781186547));
#2053=DIRECTION('',(0.,-1.,0.));
#2054=DIRECTION('center_axis',(0.,0.,1.));
#2055=DIRECTION('ref_axis',(-0.768781920329584,-0.639511031159242,0.));
#2056=DIRECTION('',(-0.128729696062163,-0.695290346079781,0.707106781186548));
#2057=DIRECTION('center_axis',(0.,0.,-1.));
#2058=DIRECTION('ref_axis',(-0.768781920329584,-0.639511031159242,0.));
#2059=DIRECTION('center_axis',(0.,0.,1.));
#2060=DIRECTION('ref_axis',(-0.768781920329584,-0.639511031159242,0.));
#2061=DIRECTION('center_axis',(0.,0.,-1.));
#2062=DIRECTION('ref_axis',(0.994407894618038,0.105607476635515,0.));
#2063=DIRECTION('center_axis',(0.,0.,-1.));
#2064=DIRECTION('ref_axis',(0.994407894618038,0.105607476635515,0.));
#2065=DIRECTION('',(-0.695290346079783,-0.128729696062162,0.707106781186546));
#2066=DIRECTION('center_axis',(0.,0.,1.));
#2067=DIRECTION('ref_axis',(0.994407894618038,0.105607476635515,0.));
#2068=DIRECTION('center_axis',(0.,0.,1.));
#2069=DIRECTION('ref_axis',(-0.639511031159243,-0.768781920329583,0.));
#2070=DIRECTION('center_axis',(0.,0.,-1.));
#2071=DIRECTION('ref_axis',(-0.639511031159243,-0.768781920329583,0.));
#2072=DIRECTION('center_axis',(0.,0.,1.));
#2073=DIRECTION('ref_axis',(-0.639511031159243,-0.768781920329583,0.));
#2074=DIRECTION('center_axis',(0.,0.,1.));
#2075=DIRECTION('ref_axis',(-0.639511031159243,0.768781920329583,0.));
#2076=DIRECTION('',(0.,0.,1.));
#2077=DIRECTION('center_axis',(0.,0.,1.));
#2078=DIRECTION('ref_axis',(-0.639511031159243,0.768781920329583,0.));
#2079=DIRECTION('center_axis',(0.,0.,1.));
#2080=DIRECTION('ref_axis',(0.105607476635514,-0.994407894618038,0.));
#2081=DIRECTION('',(0.,0.,-1.));
#2082=DIRECTION('center_axis',(0.,0.,-1.));
#2083=DIRECTION('ref_axis',(0.105607476635514,-0.994407894618038,0.));
#2084=DIRECTION('center_axis',(0.,0.,1.));
#2085=DIRECTION('ref_axis',(-0.768781920329583,0.639511031159243,0.));
#2086=DIRECTION('center_axis',(0.,0.,1.));
#2087=DIRECTION('ref_axis',(-0.768781920329583,0.639511031159243,0.));
#2088=DIRECTION('center_axis',(0.,0.,1.));
#2089=DIRECTION('ref_axis',(-0.768781920329584,-0.639511031159242,0.));
#2090=DIRECTION('',(0.,0.,1.));
#2091=DIRECTION('center_axis',(0.,0.,1.));
#2092=DIRECTION('ref_axis',(-0.768781920329584,-0.639511031159242,0.));
#2093=DIRECTION('center_axis',(0.,0.,1.));
#2094=DIRECTION('ref_axis',(0.994407894618038,0.105607476635515,0.));
#2095=DIRECTION('',(0.,0.,-1.));
#2096=DIRECTION('center_axis',(0.,0.,-1.));
#2097=DIRECTION('ref_axis',(0.994407894618038,0.105607476635515,0.));
#2098=DIRECTION('center_axis',(0.,0.,1.));
#2099=DIRECTION('ref_axis',(-0.639511031159243,-0.768781920329583,0.));
#2100=DIRECTION('center_axis',(0.,0.,1.));
#2101=DIRECTION('ref_axis',(-0.639511031159243,-0.768781920329583,0.));
#2102=DIRECTION('center_axis',(0.,0.,1.));
#2103=DIRECTION('ref_axis',(1.,0.,0.));
#2104=DIRECTION('center_axis',(0.,0.,-1.));
#2105=DIRECTION('ref_axis',(1.,0.,0.));
#2106=DIRECTION('center_axis',(0.,0.,-1.));
#2107=DIRECTION('ref_axis',(1.,0.,0.));
#2108=DIRECTION('center_axis',(0.,0.,1.));
#2109=DIRECTION('ref_axis',(1.,0.,0.));
#2110=DIRECTION('',(-0.707106781186548,-8.65956056235494E-17,-0.707106781186547));
#2111=DIRECTION('center_axis',(0.,0.,1.));
#2112=DIRECTION('ref_axis',(1.,0.,0.));
#2113=DIRECTION('center_axis',(0.,0.,-1.));
#2114=DIRECTION('ref_axis',(1.,0.,0.));
#2115=DIRECTION('',(0.,0.,-1.));
#2116=DIRECTION('center_axis',(0.,0.,1.));
#2117=DIRECTION('ref_axis',(1.,0.,0.));
#2118=DIRECTION('center_axis',(0.,0.,1.));
#2119=DIRECTION('ref_axis',(1.,0.,0.));
#2120=DIRECTION('',(0.707106781186548,8.65956056235494E-17,-0.707106781186547));
#2121=DIRECTION('center_axis',(0.,0.,1.));
#2122=DIRECTION('ref_axis',(1.,0.,0.));
#2123=DIRECTION('center_axis',(0.,0.,-1.));
#2124=DIRECTION('ref_axis',(-0.639511031159243,0.768781920329583,0.));
#2125=DIRECTION('center_axis',(0.,0.,1.));
#2126=DIRECTION('ref_axis',(0.105607476635514,-0.994407894618038,0.));
#2127=DIRECTION('center_axis',(0.,0.,-1.));
#2128=DIRECTION('ref_axis',(-0.768781920329583,0.639511031159243,0.));
#2129=DIRECTION('',(0.,1.,0.));
#2130=DIRECTION('center_axis',(0.,0.,-1.));
#2131=DIRECTION('ref_axis',(-0.768781920329584,-0.639511031159242,0.));
#2132=DIRECTION('center_axis',(0.,0.,1.));
#2133=DIRECTION('ref_axis',(0.994407894618038,0.105607476635515,0.));
#2134=DIRECTION('center_axis',(0.,0.,-1.));
#2135=DIRECTION('ref_axis',(-0.639511031159243,-0.768781920329583,0.));
#2136=DIRECTION('',(-1.,0.,0.));
#2137=DIRECTION('center_axis',(0.,0.,-1.));
#2138=DIRECTION('ref_axis',(0.639511031159242,-0.768781920329584,0.));
#2139=DIRECTION('center_axis',(0.,0.,1.));
#2140=DIRECTION('ref_axis',(-0.105607476635515,0.994407894618038,0.));
#2141=DIRECTION('center_axis',(0.,0.,-1.));
#2142=DIRECTION('ref_axis',(0.768781920329583,-0.639511031159243,0.));
#2143=DIRECTION('',(0.,-1.,0.));
#2144=DIRECTION('center_axis',(0.,0.,-1.));
#2145=DIRECTION('ref_axis',(0.768781920329583,0.639511031159243,0.));
#2146=DIRECTION('center_axis',(0.,0.,1.));
#2147=DIRECTION('ref_axis',(-0.994407894618038,-0.105607476635514,0.));
#2148=DIRECTION('center_axis',(0.,0.,-1.));
#2149=DIRECTION('ref_axis',(0.639511031159243,0.768781920329583,0.));
#2150=DIRECTION('',(1.,0.,0.));
#2151=DIRECTION('center_axis',(0.,0.,-1.));
#2152=DIRECTION('ref_axis',(-0.639511031159243,0.768781920329583,0.));
#2153=DIRECTION('',(0.,0.707106781186546,-0.707106781186549));
#2154=DIRECTION('',(0.695290346079782,-0.12872969606217,0.707106781186546));
#2155=DIRECTION('center_axis',(0.,0.707106781186547,0.707106781186548));
#2156=DIRECTION('ref_axis',(1.,0.,0.));
#2157=DIRECTION('',(0.,0.707106781186548,-0.707106781186547));
#2158=DIRECTION('center_axis',(0.,0.,-1.));
#2159=DIRECTION('ref_axis',(0.639511031159243,0.768781920329583,0.));
#2160=DIRECTION('',(0.695290346079781,0.128729696062166,-0.707106781186548));
#2161=DIRECTION('center_axis',(0.,0.,1.));
#2162=DIRECTION('ref_axis',(0.639511031159243,0.768781920329583,0.));
#2163=DIRECTION('center_axis',(0.,0.,1.));
#2164=DIRECTION('ref_axis',(-0.994407894618038,-0.105607476635514,0.));
#2165=DIRECTION('',(0.128729696062166,0.695290346079781,-0.707106781186548));
#2166=DIRECTION('center_axis',(0.,0.,-1.));
#2167=DIRECTION('ref_axis',(-0.994407894618038,-0.105607476635514,0.));
#2168=DIRECTION('center_axis',(0.,0.,-1.));
#2169=DIRECTION('ref_axis',(0.768781920329583,0.639511031159243,0.));
#2170=DIRECTION('',(0.707106781186546,0.,-0.707106781186549));
#2171=DIRECTION('center_axis',(0.,0.,1.));
#2172=DIRECTION('ref_axis',(0.768781920329583,0.639511031159243,0.));
#2173=DIRECTION('center_axis',(0.707106781186547,0.,0.707106781186548));
#2174=DIRECTION('ref_axis',(0.707106781186548,0.,-0.707106781186547));
#2175=DIRECTION('',(0.707106781186548,0.,-0.707106781186547));
#2176=DIRECTION('center_axis',(0.,0.,-1.));
#2177=DIRECTION('ref_axis',(0.768781920329583,-0.639511031159243,0.));
#2178=DIRECTION('',(0.128729696062166,-0.695290346079781,-0.707106781186548));
#2179=DIRECTION('center_axis',(0.,0.,1.));
#2180=DIRECTION('ref_axis',(0.768781920329583,-0.639511031159243,0.));
#2181=DIRECTION('center_axis',(0.,0.,1.));
#2182=DIRECTION('ref_axis',(-0.105607476635515,0.994407894618038,0.));
#2183=DIRECTION('',(0.695290346079777,-0.128729696062167,-0.707106781186552));
#2184=DIRECTION('center_axis',(0.,0.,-1.));
#2185=DIRECTION('ref_axis',(-0.105607476635515,0.994407894618038,0.));
#2186=DIRECTION('center_axis',(0.,0.,-1.));
#2187=DIRECTION('ref_axis',(0.639511031159242,-0.768781920329584,0.));
#2188=DIRECTION('',(0.,-0.707106781186548,-0.707106781186547));
#2189=DIRECTION('center_axis',(0.,0.,1.));
#2190=DIRECTION('ref_axis',(0.639511031159242,-0.768781920329584,0.));
#2191=DIRECTION('center_axis',(0.,-0.707106781186547,0.707106781186548));
#2192=DIRECTION('ref_axis',(1.,0.,0.));
#2193=DIRECTION('',(0.,-0.707106781186548,-0.707106781186547));
#2194=DIRECTION('center_axis',(0.,0.,-1.));
#2195=DIRECTION('ref_axis',(-0.639511031159243,-0.768781920329583,0.));
#2196=DIRECTION('',(-0.695290346079781,-0.128729696062166,-0.707106781186548));
#2197=DIRECTION('center_axis',(0.,0.,1.));
#2198=DIRECTION('ref_axis',(0.994407894618038,0.105607476635515,0.));
#2199=DIRECTION('',(-0.12872969606217,-0.695290346079783,-0.707106781186545));
#2200=DIRECTION('center_axis',(0.,0.,-1.));
#2201=DIRECTION('ref_axis',(-0.768781920329584,-0.639511031159242,0.));
#2202=DIRECTION('',(-0.707106781186548,0.,-0.707106781186547));
#2203=DIRECTION('center_axis',(-0.707106781186547,0.,0.707106781186548));
#2204=DIRECTION('ref_axis',(0.707106781186548,0.,0.707106781186547));
#2205=DIRECTION('',(-0.707106781186548,0.,-0.707106781186547));
#2206=DIRECTION('center_axis',(0.,0.,-1.));
#2207=DIRECTION('ref_axis',(-0.768781920329583,0.639511031159243,0.));
#2208=DIRECTION('',(-0.128729696062166,0.695290346079781,-0.707106781186548));
#2209=DIRECTION('center_axis',(0.,0.,1.));
#2210=DIRECTION('ref_axis',(0.105607476635514,-0.994407894618038,0.));
#2211=DIRECTION('center_axis',(0.,0.,1.));
#2212=DIRECTION('ref_axis',(0.639511031159242,-0.768781920329584,0.));
#2213=DIRECTION('',(0.,0.,1.));
#2214=DIRECTION('center_axis',(0.,0.,1.));
#2215=DIRECTION('ref_axis',(0.768781920329583,-0.639511031159243,0.));
#2216=DIRECTION('',(0.,0.,-1.));
#2217=DIRECTION('center_axis',(0.,0.,1.));
#2218=DIRECTION('ref_axis',(0.768781920329583,0.639511031159243,0.));
#2219=DIRECTION('',(0.,0.,1.));
#2220=DIRECTION('center_axis',(0.,0.,1.));
#2221=DIRECTION('ref_axis',(0.639511031159243,0.768781920329583,0.));
#2222=DIRECTION('',(0.,0.,-1.));
#2223=DIRECTION('center_axis',(0.,0.,1.));
#2224=DIRECTION('ref_axis',(-0.994407894618038,-0.105607476635514,0.));
#2225=DIRECTION('center_axis',(0.,0.,1.));
#2226=DIRECTION('ref_axis',(-0.105607476635515,0.994407894618038,0.));
#2227=DIRECTION('axis',(0.,0.,1.));
#2228=DIRECTION('refdir',(1.,0.,0.));
#2229=DIRECTION('center_axis',(0.,0.,1.));
#2230=DIRECTION('ref_axis',(1.,0.,0.));
#2231=DIRECTION('center_axis',(0.,0.,-1.));
#2232=DIRECTION('ref_axis',(1.,0.,0.));
#2233=DIRECTION('',(0.707106781186548,8.65956056235494E-17,-0.707106781186547));
#2234=DIRECTION('center_axis',(0.,0.,1.));
#2235=DIRECTION('ref_axis',(1.,0.,0.));
#2236=DIRECTION('center_axis',(0.,0.,1.));
#2237=DIRECTION('ref_axis',(1.,0.,0.));
#2238=DIRECTION('center_axis',(0.,0.,1.));
#2239=DIRECTION('ref_axis',(1.,0.,0.));
#2240=DIRECTION('',(0.,0.,-1.));
#2241=DIRECTION('center_axis',(0.,0.,1.));
#2242=DIRECTION('ref_axis',(1.,0.,0.));
#2243=DIRECTION('center_axis',(0.,0.,-1.));
#2244=DIRECTION('ref_axis',(1.,0.,0.));
#2245=DIRECTION('center_axis',(0.,0.,-1.));
#2246=DIRECTION('ref_axis',(1.,0.,0.));
#2247=DIRECTION('',(-0.707106781186548,-8.65956056235494E-17,-0.707106781186548));
#2248=DIRECTION('center_axis',(0.,0.,1.));
#2249=DIRECTION('ref_axis',(1.,0.,0.));
#2250=DIRECTION('axis',(0.,0.,1.));
#2251=DIRECTION('refdir',(1.,0.,0.));
#2252=DIRECTION('center_axis',(6.12323399573677E-17,0.,1.));
#2253=DIRECTION('ref_axis',(1.,0.,0.));
#2254=DIRECTION('center_axis',(1.22464679914735E-16,-1.,0.));
#2255=DIRECTION('ref_axis',(-1.,-1.22464679914735E-16,0.));
#2256=DIRECTION('axis',(0.,0.,1.));
#2257=DIRECTION('refdir',(1.,0.,0.));
#2258=DIRECTION('center_axis',(-1.,0.,0.));
#2259=DIRECTION('ref_axis',(0.,0.,1.));
#2260=DIRECTION('center_axis',(1.,0.,0.));
#2261=DIRECTION('ref_axis',(0.,0.,-1.));
#2262=DIRECTION('center_axis',(1.,0.,0.));
#2263=DIRECTION('ref_axis',(0.,1.,0.));
#2264=DIRECTION('center_axis',(1.,0.,0.));
#2265=DIRECTION('ref_axis',(0.,0.,-1.));
#2266=DIRECTION('',(-0.707106781186548,0.707106781186547,8.65956056235493E-17));
#2267=DIRECTION('center_axis',(1.,0.,0.));
#2268=DIRECTION('ref_axis',(0.,1.,0.));
#2269=DIRECTION('center_axis',(1.,0.,0.));
#2270=DIRECTION('ref_axis',(0.,0.,-1.));
#2271=DIRECTION('',(-1.,0.,0.));
#2272=DIRECTION('center_axis',(-1.,0.,0.));
#2273=DIRECTION('ref_axis',(0.,1.,0.));
#2274=DIRECTION('center_axis',(1.,0.,0.));
#2275=DIRECTION('ref_axis',(0.,0.,-1.));
#2276=DIRECTION('',(-0.707106781186548,-0.707106781186547,-8.65956056235493E-17));
#2277=DIRECTION('center_axis',(1.,0.,0.));
#2278=DIRECTION('ref_axis',(0.,0.,-1.));
#2279=DIRECTION('',(0.,0.,1.));
#2280=DIRECTION('',(1.,0.,0.));
#2281=DIRECTION('',(0.,0.,1.));
#2282=DIRECTION('',(1.,0.,0.));
#2283=DIRECTION('',(0.,0.,1.));
#2284=DIRECTION('',(1.,0.,0.));
#2285=DIRECTION('',(0.,0.,1.));
#2286=DIRECTION('',(1.,0.,0.));
#2287=DIRECTION('',(0.,0.,1.));
#2288=DIRECTION('',(1.,0.,0.));
#2289=DIRECTION('',(0.,0.,1.));
#2290=DIRECTION('',(1.,0.,0.));
#2291=DIRECTION('',(0.,0.,1.));
#2292=DIRECTION('',(1.,0.,0.));
#2293=DIRECTION('',(0.,0.,1.));
#2294=DIRECTION('',(6.12323399573677E-17,1.,0.));
#2295=DIRECTION('',(0.,0.,1.));
#2296=DIRECTION('',(6.12323399573677E-17,1.,0.));
#2297=DIRECTION('',(0.,0.,1.));
#2298=DIRECTION('',(-1.,1.22464679914735E-16,0.));
#2299=DIRECTION('',(0.,0.,1.));
#2300=DIRECTION('',(-1.,1.22464679914735E-16,0.));
#2301=DIRECTION('',(0.,0.,1.));
#2302=DIRECTION('',(-1.83697019872103E-16,-1.,0.));
#2303=DIRECTION('',(0.,0.,1.));
#2304=DIRECTION('',(-1.83697019872103E-16,-1.,0.));
#2305=CARTESIAN_POINT('',(0.,0.,0.));
#2306=CARTESIAN_POINT('',(0.,0.,0.));
#2307=CARTESIAN_POINT('Origin',(26.9,-2.,5.3));
#2308=CARTESIAN_POINT('',(27.,-2.,6.75));
#2309=CARTESIAN_POINT('Origin',(27.,-2.,5.3));
#2310=CARTESIAN_POINT('',(26.8,-2.,6.55));
#2311=CARTESIAN_POINT('',(26.9,-2.,6.65));
#2312=CARTESIAN_POINT('Origin',(26.8,-2.,5.3));
#2313=CARTESIAN_POINT('Origin',(27.,-7.97967105517398,0.));
#2314=CARTESIAN_POINT('',(27.,6.25103652921323,0.4));
#2315=CARTESIAN_POINT('',(27.,-6.25103652921323,0.4));
#2316=CARTESIAN_POINT('',(27.,-3.98983552758699,0.4));
#2317=CARTESIAN_POINT('',(27.,6.25103652921323,8.2));
#2318=CARTESIAN_POINT('',(27.,6.25103652921323,0.));
#2319=CARTESIAN_POINT('',(27.,-6.25103652921323,8.2));
#2320=CARTESIAN_POINT('',(27.,-3.98983552758699,8.2));
#2321=CARTESIAN_POINT('',(27.,-6.25103652921323,0.));
#2322=CARTESIAN_POINT('',(27.,2.,6.75));
#2323=CARTESIAN_POINT('Origin',(27.,2.,5.3));
#2324=CARTESIAN_POINT('Origin',(0.,-2.,5.3));
#2325=CARTESIAN_POINT('',(24.9186985827943,-0.75,5.3));
#2326=CARTESIAN_POINT('',(24.372281323269,-2.,6.55));
#2327=CARTESIAN_POINT('Ctrl Pts',(24.9186985827943,-0.75,5.3));
#2328=CARTESIAN_POINT('Ctrl Pts',(24.9186985827943,-0.75,5.45557706538823));
#2329=CARTESIAN_POINT('Ctrl Pts',(24.9123746835565,-0.780900542172469,5.62135879792505));
#2330=CARTESIAN_POINT('Ctrl Pts',(24.8815010802748,-0.905294021223847,5.92537474512899));
#2331=CARTESIAN_POINT('Ctrl Pts',(24.8563182098205,-0.998771663818447,6.06355058537597));
#2332=CARTESIAN_POINT('Ctrl Pts',(24.78127088064,-1.22443201701213,6.29525819606588));
#2333=CARTESIAN_POINT('Ctrl Pts',(24.7232785375987,-1.37524312511396,6.39595782382434));
#2334=CARTESIAN_POINT('Ctrl Pts',(24.5694895702423,-1.69087323617109,6.52306381241391));
#2335=CARTESIAN_POINT('Ctrl Pts',(24.4731108768197,-1.85519457825137,6.55));
#2336=CARTESIAN_POINT('Ctrl Pts',(24.372281323269,-2.,6.55));
#2337=CARTESIAN_POINT('Ctrl Pts',(24.372281323269,-2.,6.55));
#2338=CARTESIAN_POINT('Ctrl Pts',(24.2385424047286,-2.19206789895891,6.55));
#2339=CARTESIAN_POINT('Ctrl Pts',(24.0765750988521,-2.38072616471554,6.50435864359466));
#2340=CARTESIAN_POINT('Ctrl Pts',(23.7307236627921,-2.70748360064366,6.34637446065785));
#2341=CARTESIAN_POINT('Ctrl Pts',(23.5468663875633,-2.84596078128561,6.23475573757803));
#2342=CARTESIAN_POINT('Ctrl Pts',(23.2511744930699,-3.03425420344229,6.01333284729064));
#2343=CARTESIAN_POINT('Ctrl Pts',(23.1129712312086,-3.10865620052542,5.89516586902311));
#2344=CARTESIAN_POINT('Ctrl Pts',(22.9447171723108,-3.18851767079192,5.69387466967946));
#2345=CARTESIAN_POINT('Ctrl Pts',(22.8954952065846,-3.2100076151372,5.62308391879915));
#2346=CARTESIAN_POINT('Ctrl Pts',(22.8227994048359,-3.24064153091951,5.47120219564432));
#2347=CARTESIAN_POINT('Ctrl Pts',(22.7990381056767,-3.25,5.39029234212096));
#2348=CARTESIAN_POINT('Ctrl Pts',(22.7990381056767,-3.25,5.20970765787903));
#2349=CARTESIAN_POINT('Ctrl Pts',(22.8227994048359,-3.24064153091951,5.12879780435568));
#2350=CARTESIAN_POINT('Ctrl Pts',(22.8954952065846,-3.2100076151372,4.97691608120085));
#2351=CARTESIAN_POINT('Ctrl Pts',(22.9447171723108,-3.18851767079192,4.90612533032054));
#2352=CARTESIAN_POINT('Ctrl Pts',(23.1129712312086,-3.10865620052542,4.70483413097689));
#2353=CARTESIAN_POINT('Ctrl Pts',(23.2511744930699,-3.03425420344229,4.58666715270936));
#2354=CARTESIAN_POINT('Ctrl Pts',(23.5468663875633,-2.84596078128561,4.36524426242197));
#2355=CARTESIAN_POINT('Ctrl Pts',(23.7307236627921,-2.70748360064366,4.25362553934216));
#2356=CARTESIAN_POINT('Ctrl Pts',(24.0765750988521,-2.38072616471554,4.09564135640534));
#2357=CARTESIAN_POINT('Ctrl Pts',(24.2385424047286,-2.19206789895891,4.05));
#2358=CARTESIAN_POINT('Ctrl Pts',(24.4731108768197,-1.85519457825137,4.05));
#2359=CARTESIAN_POINT('Ctrl Pts',(24.5694895702423,-1.69087323617109,4.07693618758609));
#2360=CARTESIAN_POINT('Ctrl Pts',(24.7232785375987,-1.37524312511396,4.20404217617566));
#2361=CARTESIAN_POINT('Ctrl Pts',(24.7812708806401,-1.22443201701213,4.30474180393412));
#2362=CARTESIAN_POINT('Ctrl Pts',(24.8563182098205,-0.998771663818447,4.53644941462403));
#2363=CARTESIAN_POINT('Ctrl Pts',(24.8815010802748,-0.905294021223847,4.67462525487101));
#2364=CARTESIAN_POINT('Ctrl Pts',(24.9123746835565,-0.780900542172468,4.97864120207495));
#2365=CARTESIAN_POINT('Ctrl Pts',(24.9186985827943,-0.75,5.14442293461177));
#2366=CARTESIAN_POINT('Ctrl Pts',(24.9186985827943,-0.75,5.3));
#2367=CARTESIAN_POINT('',(0.,-2.,6.55));
#2368=CARTESIAN_POINT('Origin',(-26.9,-2.,5.3));
#2369=CARTESIAN_POINT('',(-27.,-2.,6.75));
#2370=CARTESIAN_POINT('Origin',(-27.,-2.,5.3));
#2371=CARTESIAN_POINT('',(-26.8,-2.,6.55));
#2372=CARTESIAN_POINT('',(-26.9,-2.,6.65));
#2373=CARTESIAN_POINT('Origin',(-26.8,-2.,5.3));
#2374=CARTESIAN_POINT('Origin',(-27.,7.97967105517399,0.));
#2375=CARTESIAN_POINT('',(-27.,-6.25103652921323,0.4));
#2376=CARTESIAN_POINT('',(-27.,6.25103652921323,0.4));
#2377=CARTESIAN_POINT('',(-27.,3.98983552758699,0.4));
#2378=CARTESIAN_POINT('',(-27.,-6.25103652921323,8.2));
#2379=CARTESIAN_POINT('',(-27.,-6.25103652921323,0.));
#2380=CARTESIAN_POINT('',(-27.,6.25103652921323,8.2));
#2381=CARTESIAN_POINT('',(-27.,3.98983552758699,8.2));
#2382=CARTESIAN_POINT('',(-27.,6.25103652921323,0.));
#2383=CARTESIAN_POINT('',(-27.,2.,6.75));
#2384=CARTESIAN_POINT('Origin',(-27.,2.,5.3));
#2385=CARTESIAN_POINT('Origin',(0.,-2.,5.3));
#2386=CARTESIAN_POINT('',(-24.372281323269,-2.,6.55));
#2387=CARTESIAN_POINT('',(0.,-2.,6.55));
#2388=CARTESIAN_POINT('',(-24.9186985827943,-0.75,5.3));
#2389=CARTESIAN_POINT('Ctrl Pts',(-24.9186985827943,-0.75,5.3));
#2390=CARTESIAN_POINT('Ctrl Pts',(-24.9186985827943,-0.75,5.14442293461177));
#2391=CARTESIAN_POINT('Ctrl Pts',(-24.9123746835565,-0.780900542172468,
4.97864120207495));
#2392=CARTESIAN_POINT('Ctrl Pts',(-24.8815010802748,-0.905294021223847,
4.67462525487101));
#2393=CARTESIAN_POINT('Ctrl Pts',(-24.8563182098205,-0.998771663818447,
4.53644941462403));
#2394=CARTESIAN_POINT('Ctrl Pts',(-24.78127088064,-1.22443201701213,4.30474180393412));
#2395=CARTESIAN_POINT('Ctrl Pts',(-24.7232785375987,-1.37524312511397,4.20404217617566));
#2396=CARTESIAN_POINT('Ctrl Pts',(-24.5694895702423,-1.69087323617109,4.07693618758609));
#2397=CARTESIAN_POINT('Ctrl Pts',(-24.4731108768197,-1.85519457825137,4.05));
#2398=CARTESIAN_POINT('Ctrl Pts',(-24.2385424047286,-2.19206789895891,4.05));
#2399=CARTESIAN_POINT('Ctrl Pts',(-24.0765750988521,-2.38072616471554,4.09564135640534));
#2400=CARTESIAN_POINT('Ctrl Pts',(-23.7307236627921,-2.70748360064366,4.25362553934216));
#2401=CARTESIAN_POINT('Ctrl Pts',(-23.5468663875633,-2.84596078128561,4.36524426242197));
#2402=CARTESIAN_POINT('Ctrl Pts',(-23.2511744930699,-3.03425420344229,4.58666715270936));
#2403=CARTESIAN_POINT('Ctrl Pts',(-23.1129712312086,-3.10865620052542,4.70483413097689));
#2404=CARTESIAN_POINT('Ctrl Pts',(-22.9447171723108,-3.18851767079192,4.90612533032054));
#2405=CARTESIAN_POINT('Ctrl Pts',(-22.8954952065846,-3.2100076151372,4.97691608120085));
#2406=CARTESIAN_POINT('Ctrl Pts',(-22.8227994048359,-3.24064153091951,5.12879780435568));
#2407=CARTESIAN_POINT('Ctrl Pts',(-22.7990381056767,-3.25,5.20970765787904));
#2408=CARTESIAN_POINT('Ctrl Pts',(-22.7990381056767,-3.25,5.39029234212096));
#2409=CARTESIAN_POINT('Ctrl Pts',(-22.8227994048359,-3.24064153091951,5.47120219564432));
#2410=CARTESIAN_POINT('Ctrl Pts',(-22.8954952065846,-3.2100076151372,5.62308391879915));
#2411=CARTESIAN_POINT('Ctrl Pts',(-22.9447171723108,-3.18851767079192,5.69387466967946));
#2412=CARTESIAN_POINT('Ctrl Pts',(-23.1129712312086,-3.10865620052542,5.89516586902311));
#2413=CARTESIAN_POINT('Ctrl Pts',(-23.2511744930699,-3.03425420344229,6.01333284729064));
#2414=CARTESIAN_POINT('Ctrl Pts',(-23.5468663875633,-2.84596078128561,6.23475573757803));
#2415=CARTESIAN_POINT('Ctrl Pts',(-23.7307236627921,-2.70748360064366,6.34637446065785));
#2416=CARTESIAN_POINT('Ctrl Pts',(-24.0765750988521,-2.38072616471554,6.50435864359466));
#2417=CARTESIAN_POINT('Ctrl Pts',(-24.2385424047286,-2.19206789895891,6.55));
#2418=CARTESIAN_POINT('Ctrl Pts',(-24.372281323269,-2.,6.55));
#2419=CARTESIAN_POINT('Ctrl Pts',(-24.372281323269,-2.,6.55));
#2420=CARTESIAN_POINT('Ctrl Pts',(-24.4731108768197,-1.85519457825137,6.55));
#2421=CARTESIAN_POINT('Ctrl Pts',(-24.5694895702423,-1.69087323617109,6.52306381241391));
#2422=CARTESIAN_POINT('Ctrl Pts',(-24.7232785375987,-1.37524312511397,6.39595782382434));
#2423=CARTESIAN_POINT('Ctrl Pts',(-24.78127088064,-1.22443201701213,6.29525819606588));
#2424=CARTESIAN_POINT('Ctrl Pts',(-24.8563182098205,-0.998771663818447,
6.06355058537597));
#2425=CARTESIAN_POINT('Ctrl Pts',(-24.8815010802748,-0.905294021223847,
5.92537474512899));
#2426=CARTESIAN_POINT('Ctrl Pts',(-24.9123746835565,-0.780900542172469,
5.62135879792505));
#2427=CARTESIAN_POINT('Ctrl Pts',(-24.9186985827943,-0.75,5.45557706538823));
#2428=CARTESIAN_POINT('Ctrl Pts',(-24.9186985827943,-0.75,5.3));
#2429=CARTESIAN_POINT('Origin',(26.9,2.,5.3));
#2430=CARTESIAN_POINT('',(26.8,2.,6.55));
#2431=CARTESIAN_POINT('',(26.9,2.,6.65));
#2432=CARTESIAN_POINT('Origin',(26.8,2.,5.3));
#2433=CARTESIAN_POINT('Origin',(0.,2.,5.3));
#2434=CARTESIAN_POINT('',(22.7990381056767,3.25,5.3));
#2435=CARTESIAN_POINT('',(24.372281323269,2.,6.55));
#2436=CARTESIAN_POINT('Ctrl Pts',(22.7990381056767,3.25,5.3));
#2437=CARTESIAN_POINT('Ctrl Pts',(22.7990381056767,3.25,5.39029234212097));
#2438=CARTESIAN_POINT('Ctrl Pts',(22.8227994048359,3.24064153091951,5.47120219564433));
#2439=CARTESIAN_POINT('Ctrl Pts',(22.8954952065846,3.2100076151372,5.62308391879915));
#2440=CARTESIAN_POINT('Ctrl Pts',(22.9447171723108,3.18851767079192,5.69387466967946));
#2441=CARTESIAN_POINT('Ctrl Pts',(23.1129712312086,3.10865620052542,5.89516586902311));
#2442=CARTESIAN_POINT('Ctrl Pts',(23.2511744930699,3.03425420344229,6.01333284729064));
#2443=CARTESIAN_POINT('Ctrl Pts',(23.5468663875633,2.84596078128561,6.23475573757803));
#2444=CARTESIAN_POINT('Ctrl Pts',(23.7307236627921,2.70748360064366,6.34637446065785));
#2445=CARTESIAN_POINT('Ctrl Pts',(24.0765750988521,2.38072616471554,6.50435864359466));
#2446=CARTESIAN_POINT('Ctrl Pts',(24.2385424047286,2.19206789895891,6.55));
#2447=CARTESIAN_POINT('Ctrl Pts',(24.372281323269,2.,6.55));
#2448=CARTESIAN_POINT('Ctrl Pts',(24.372281323269,2.,6.55));
#2449=CARTESIAN_POINT('Ctrl Pts',(24.4731108768197,1.85519457825136,6.55));
#2450=CARTESIAN_POINT('Ctrl Pts',(24.5694895702423,1.69087323617109,6.52306381241391));
#2451=CARTESIAN_POINT('Ctrl Pts',(24.7232785375987,1.37524312511396,6.39595782382434));
#2452=CARTESIAN_POINT('Ctrl Pts',(24.7812708806401,1.22443201701213,6.29525819606588));
#2453=CARTESIAN_POINT('Ctrl Pts',(24.8563182098205,0.998771663818447,6.06355058537597));
#2454=CARTESIAN_POINT('Ctrl Pts',(24.8815010802748,0.905294021223848,5.92537474512899));
#2455=CARTESIAN_POINT('Ctrl Pts',(24.9123746835565,0.780900542172469,5.62135879792505));
#2456=CARTESIAN_POINT('Ctrl Pts',(24.9186985827943,0.75,5.45557706538823));
#2457=CARTESIAN_POINT('Ctrl Pts',(24.9186985827943,0.75,5.14442293461177));
#2458=CARTESIAN_POINT('Ctrl Pts',(24.9123746835565,0.780900542172469,4.97864120207495));
#2459=CARTESIAN_POINT('Ctrl Pts',(24.8815010802748,0.905294021223848,4.67462525487101));
#2460=CARTESIAN_POINT('Ctrl Pts',(24.8563182098205,0.998771663818447,4.53644941462403));
#2461=CARTESIAN_POINT('Ctrl Pts',(24.78127088064,1.22443201701213,4.30474180393412));
#2462=CARTESIAN_POINT('Ctrl Pts',(24.7232785375987,1.37524312511397,4.20404217617566));
#2463=CARTESIAN_POINT('Ctrl Pts',(24.5694895702423,1.69087323617109,4.07693618758609));
#2464=CARTESIAN_POINT('Ctrl Pts',(24.4731108768197,1.85519457825137,4.05));
#2465=CARTESIAN_POINT('Ctrl Pts',(24.2385424047286,2.19206789895891,4.05));
#2466=CARTESIAN_POINT('Ctrl Pts',(24.0765750988521,2.38072616471554,4.09564135640534));
#2467=CARTESIAN_POINT('Ctrl Pts',(23.7307236627921,2.70748360064366,4.25362553934216));
#2468=CARTESIAN_POINT('Ctrl Pts',(23.5468663875633,2.84596078128561,4.36524426242197));
#2469=CARTESIAN_POINT('Ctrl Pts',(23.2511744930699,3.03425420344229,4.58666715270936));
#2470=CARTESIAN_POINT('Ctrl Pts',(23.1129712312086,3.10865620052542,4.70483413097689));
#2471=CARTESIAN_POINT('Ctrl Pts',(22.9447171723108,3.18851767079192,4.90612533032054));
#2472=CARTESIAN_POINT('Ctrl Pts',(22.8954952065846,3.2100076151372,4.97691608120085));
#2473=CARTESIAN_POINT('Ctrl Pts',(22.8227994048359,3.24064153091951,5.12879780435568));
#2474=CARTESIAN_POINT('Ctrl Pts',(22.7990381056767,3.25,5.20970765787903));
#2475=CARTESIAN_POINT('Ctrl Pts',(22.7990381056767,3.25,5.3));
#2476=CARTESIAN_POINT('',(0.,2.,6.55));
#2477=CARTESIAN_POINT('Origin',(-26.9,2.,5.3));
#2478=CARTESIAN_POINT('',(-26.8,2.,6.55));
#2479=CARTESIAN_POINT('',(-26.9,2.,6.65));
#2480=CARTESIAN_POINT('Origin',(-26.8,2.,5.3));
#2481=CARTESIAN_POINT('Origin',(0.,2.,5.3));
#2482=CARTESIAN_POINT('',(-24.372281323269,2.,6.55));
#2483=CARTESIAN_POINT('',(0.,2.,6.55));
#2484=CARTESIAN_POINT('',(-22.7990381056767,3.25,5.3));
#2485=CARTESIAN_POINT('Ctrl Pts',(-22.7990381056767,3.25,5.3));
#2486=CARTESIAN_POINT('Ctrl Pts',(-22.7990381056767,3.25,5.20970765787904));
#2487=CARTESIAN_POINT('Ctrl Pts',(-22.8227994048359,3.24064153091951,5.12879780435568));
#2488=CARTESIAN_POINT('Ctrl Pts',(-22.8954952065846,3.2100076151372,4.97691608120085));
#2489=CARTESIAN_POINT('Ctrl Pts',(-22.9447171723108,3.18851767079192,4.90612533032054));
#2490=CARTESIAN_POINT('Ctrl Pts',(-23.1129712312086,3.10865620052542,4.70483413097689));
#2491=CARTESIAN_POINT('Ctrl Pts',(-23.2511744930699,3.03425420344229,4.58666715270936));
#2492=CARTESIAN_POINT('Ctrl Pts',(-23.5468663875633,2.84596078128561,4.36524426242197));
#2493=CARTESIAN_POINT('Ctrl Pts',(-23.7307236627921,2.70748360064366,4.25362553934216));
#2494=CARTESIAN_POINT('Ctrl Pts',(-24.0765750988521,2.38072616471554,4.09564135640534));
#2495=CARTESIAN_POINT('Ctrl Pts',(-24.2385424047286,2.19206789895891,4.05));
#2496=CARTESIAN_POINT('Ctrl Pts',(-24.4731108768197,1.85519457825137,4.05));
#2497=CARTESIAN_POINT('Ctrl Pts',(-24.5694895702423,1.69087323617109,4.07693618758609));
#2498=CARTESIAN_POINT('Ctrl Pts',(-24.7232785375987,1.37524312511396,4.20404217617566));
#2499=CARTESIAN_POINT('Ctrl Pts',(-24.7812708806401,1.22443201701213,4.30474180393412));
#2500=CARTESIAN_POINT('Ctrl Pts',(-24.8563182098205,0.998771663818447,4.53644941462403));
#2501=CARTESIAN_POINT('Ctrl Pts',(-24.8815010802748,0.905294021223848,4.67462525487101));
#2502=CARTESIAN_POINT('Ctrl Pts',(-24.9123746835565,0.780900542172469,4.97864120207495));
#2503=CARTESIAN_POINT('Ctrl Pts',(-24.9186985827943,0.75,5.14442293461177));
#2504=CARTESIAN_POINT('Ctrl Pts',(-24.9186985827943,0.75,5.45557706538823));
#2505=CARTESIAN_POINT('Ctrl Pts',(-24.9123746835565,0.780900542172468,5.62135879792505));
#2506=CARTESIAN_POINT('Ctrl Pts',(-24.8815010802748,0.905294021223847,5.92537474512899));
#2507=CARTESIAN_POINT('Ctrl Pts',(-24.8563182098205,0.998771663818447,6.06355058537597));
#2508=CARTESIAN_POINT('Ctrl Pts',(-24.7812708806401,1.22443201701213,6.29525819606588));
#2509=CARTESIAN_POINT('Ctrl Pts',(-24.7232785375987,1.37524312511396,6.39595782382434));
#2510=CARTESIAN_POINT('Ctrl Pts',(-24.5694895702423,1.69087323617109,6.52306381241391));
#2511=CARTESIAN_POINT('Ctrl Pts',(-24.4731108768197,1.85519457825136,6.55));
#2512=CARTESIAN_POINT('Ctrl Pts',(-24.372281323269,2.,6.55));
#2513=CARTESIAN_POINT('Ctrl Pts',(-24.372281323269,2.,6.55));
#2514=CARTESIAN_POINT('Ctrl Pts',(-24.2385424047286,2.19206789895891,6.55));
#2515=CARTESIAN_POINT('Ctrl Pts',(-24.0765750988521,2.38072616471554,6.50435864359466));
#2516=CARTESIAN_POINT('Ctrl Pts',(-23.7307236627921,2.70748360064366,6.34637446065785));
#2517=CARTESIAN_POINT('Ctrl Pts',(-23.5468663875633,2.84596078128561,6.23475573757803));
#2518=CARTESIAN_POINT('Ctrl Pts',(-23.2511744930699,3.03425420344229,6.01333284729064));
#2519=CARTESIAN_POINT('Ctrl Pts',(-23.1129712312086,3.10865620052542,5.89516586902311));
#2520=CARTESIAN_POINT('Ctrl Pts',(-22.9447171723108,3.18851767079192,5.69387466967946));
#2521=CARTESIAN_POINT('Ctrl Pts',(-22.8954952065846,3.2100076151372,5.62308391879915));
#2522=CARTESIAN_POINT('Ctrl Pts',(-22.8227994048359,3.24064153091951,5.47120219564432));
#2523=CARTESIAN_POINT('Ctrl Pts',(-22.7990381056767,3.25,5.39029234212096));
#2524=CARTESIAN_POINT('Ctrl Pts',(-22.7990381056767,3.25,5.3));
#2525=CARTESIAN_POINT('Origin',(-2.,26.9,5.3));
#2526=CARTESIAN_POINT('',(-3.45,27.,5.3));
#2527=CARTESIAN_POINT('Origin',(-2.,27.,5.3));
#2528=CARTESIAN_POINT('',(-3.25,26.8,5.3));
#2529=CARTESIAN_POINT('',(-3.35,26.9,5.3));
#2530=CARTESIAN_POINT('Origin',(-2.,26.8,5.3));
#2531=CARTESIAN_POINT('Origin',(7.97967105517399,27.,0.));
#2532=CARTESIAN_POINT('',(-6.25103652921323,27.,0.4));
#2533=CARTESIAN_POINT('',(6.25103652921323,27.,0.4));
#2534=CARTESIAN_POINT('',(3.98983552758699,27.,0.4));
#2535=CARTESIAN_POINT('',(-6.25103652921323,27.,8.2));
#2536=CARTESIAN_POINT('',(-6.25103652921323,27.,0.));
#2537=CARTESIAN_POINT('',(6.25103652921323,27.,8.2));
#2538=CARTESIAN_POINT('',(3.98983552758699,27.,8.2));
#2539=CARTESIAN_POINT('',(6.25103652921323,27.,0.));
#2540=CARTESIAN_POINT('',(0.55,27.,5.3));
#2541=CARTESIAN_POINT('Origin',(2.,27.,5.3));
#2542=CARTESIAN_POINT('Origin',(-2.,0.,5.3));
#2543=CARTESIAN_POINT('',(-3.25,13.1029576813787,5.3));
#2544=CARTESIAN_POINT('Ctrl Pts',(-3.25,13.1029576813787,5.3));
#2545=CARTESIAN_POINT('Ctrl Pts',(-3.25,13.1029576813787,5.45705900752669));
#2546=CARTESIAN_POINT('Ctrl Pts',(-3.21857778155664,13.1108737267815,5.6242083709253));
#2547=CARTESIAN_POINT('Ctrl Pts',(-3.09176308346025,13.1413566197491,5.93094872999216));
#2548=CARTESIAN_POINT('Ctrl Pts',(-2.99640130889512,13.163742383297,6.07057038726816));
#2549=CARTESIAN_POINT('Ctrl Pts',(-2.77577516736032,13.2120416331141,6.29277806157361));
#2550=CARTESIAN_POINT('Ctrl Pts',(-2.6349594886099,13.2412866081987,6.38963814030342));
#2551=CARTESIAN_POINT('Ctrl Pts',(-2.32609557960331,13.2990210880236,6.51825552186166));
#2552=CARTESIAN_POINT('Ctrl Pts',(-2.15801374389282,13.3273592779611,6.55));
#2553=CARTESIAN_POINT('Ctrl Pts',(-1.84370531767661,13.3744430502294,6.55));
#2554=CARTESIAN_POINT('Ctrl Pts',(-1.67642144832972,13.3964062370615,6.51887197142702));
#2555=CARTESIAN_POINT('Ctrl Pts',(-1.36798879559555,13.431407059342,6.39128997486268));
#2556=CARTESIAN_POINT('Ctrl Pts',(-1.22686674457499,13.4446014654523,6.29481443961593));
#2557=CARTESIAN_POINT('Ctrl Pts',(-1.00475112921042,13.4630160869044,6.07233750789797));
#2558=CARTESIAN_POINT('Ctrl Pts',(-0.908716991768158,13.4695324913417,5.93192759707115));
#2559=CARTESIAN_POINT('Ctrl Pts',(-0.781341233035619,13.4775212102557,5.62419425457921));
#2560=CARTESIAN_POINT('Ctrl Pts',(-0.75,13.4791505667086,5.4568747590473));
#2561=CARTESIAN_POINT('Ctrl Pts',(-0.75,13.4791505667086,5.1431252409527));
#2562=CARTESIAN_POINT('Ctrl Pts',(-0.78134123303562,13.4775212102557,4.97580574542079));
#2563=CARTESIAN_POINT('Ctrl Pts',(-0.908716991768159,13.4695324913417,4.66807240292884));
#2564=CARTESIAN_POINT('Ctrl Pts',(-1.00475112921042,13.4630160869044,4.52766249210203));
#2565=CARTESIAN_POINT('Ctrl Pts',(-1.22686674457499,13.4446014654523,4.30518556038407));
#2566=CARTESIAN_POINT('Ctrl Pts',(-1.36798879559555,13.431407059342,4.20871002513732));
#2567=CARTESIAN_POINT('Ctrl Pts',(-1.67642144832971,13.3964062370615,4.08112802857298));
#2568=CARTESIAN_POINT('Ctrl Pts',(-1.84370531767661,13.3744430502294,4.05));
#2569=CARTESIAN_POINT('Ctrl Pts',(-2.15801374389282,13.3273592779611,4.05));
#2570=CARTESIAN_POINT('Ctrl Pts',(-2.32609557960331,13.2990210880236,4.08174447813834));
#2571=CARTESIAN_POINT('Ctrl Pts',(-2.6349594886099,13.2412866081987,4.21036185969659));
#2572=CARTESIAN_POINT('Ctrl Pts',(-2.77577516736032,13.2120416331141,4.30722193842639));
#2573=CARTESIAN_POINT('Ctrl Pts',(-2.99640130889512,13.163742383297,4.52942961273184));
#2574=CARTESIAN_POINT('Ctrl Pts',(-3.09176308346025,13.1413566197491,4.66905127000784));
#2575=CARTESIAN_POINT('Ctrl Pts',(-3.21857778155663,13.1108737267815,4.97579162907471));
#2576=CARTESIAN_POINT('Ctrl Pts',(-3.25,13.1029576813787,5.1429409924733));
#2577=CARTESIAN_POINT('Ctrl Pts',(-3.25,13.1029576813787,5.3));
#2578=CARTESIAN_POINT('',(-3.25,0.,5.3));
#2579=CARTESIAN_POINT('Origin',(-2.,-26.9,5.3));
#2580=CARTESIAN_POINT('',(-3.45,-27.,5.3));
#2581=CARTESIAN_POINT('Origin',(-2.,-27.,5.3));
#2582=CARTESIAN_POINT('',(-3.25,-26.8,5.3));
#2583=CARTESIAN_POINT('',(-3.35,-26.9,5.3));
#2584=CARTESIAN_POINT('Origin',(-2.,-26.8,5.3));
#2585=CARTESIAN_POINT('Origin',(-7.97967105517399,-27.,0.));
#2586=CARTESIAN_POINT('',(6.25103652921323,-27.,0.4));
#2587=CARTESIAN_POINT('',(-6.25103652921324,-27.,0.4));
#2588=CARTESIAN_POINT('',(-3.98983552758699,-27.,0.4));
#2589=CARTESIAN_POINT('',(6.25103652921323,-27.,8.2));
#2590=CARTESIAN_POINT('',(6.25103652921323,-27.,0.));
#2591=CARTESIAN_POINT('',(-6.25103652921324,-27.,8.2));
#2592=CARTESIAN_POINT('',(-3.98983552758699,-27.,8.2));
#2593=CARTESIAN_POINT('',(-6.25103652921324,-27.,0.));
#2594=CARTESIAN_POINT('',(0.55,-27.,5.3));
#2595=CARTESIAN_POINT('Origin',(2.,-27.,5.3));
#2596=CARTESIAN_POINT('Origin',(-2.,0.,5.3));
#2597=CARTESIAN_POINT('',(-3.25,-13.1029576813787,5.3));
#2598=CARTESIAN_POINT('',(-3.25,0.,5.3));
#2599=CARTESIAN_POINT('Ctrl Pts',(-3.25,-13.1029576813787,5.3));
#2600=CARTESIAN_POINT('Ctrl Pts',(-3.25,-13.1029576813787,5.1429409924733));
#2601=CARTESIAN_POINT('Ctrl Pts',(-3.21857778155663,-13.1108737267815,4.97579162907471));
#2602=CARTESIAN_POINT('Ctrl Pts',(-3.09176308346025,-13.1413566197491,4.66905127000784));
#2603=CARTESIAN_POINT('Ctrl Pts',(-2.99640130889512,-13.163742383297,4.52942961273184));
#2604=CARTESIAN_POINT('Ctrl Pts',(-2.77577516736032,-13.2120416331141,4.30722193842639));
#2605=CARTESIAN_POINT('Ctrl Pts',(-2.6349594886099,-13.2412866081987,4.21036185969658));
#2606=CARTESIAN_POINT('Ctrl Pts',(-2.32609557960331,-13.2990210880236,4.08174447813834));
#2607=CARTESIAN_POINT('Ctrl Pts',(-2.15801374389282,-13.3273592779611,4.05));
#2608=CARTESIAN_POINT('Ctrl Pts',(-1.84370531767661,-13.3744430502294,4.05));
#2609=CARTESIAN_POINT('Ctrl Pts',(-1.67642144832971,-13.3964062370615,4.08112802857298));
#2610=CARTESIAN_POINT('Ctrl Pts',(-1.36798879559555,-13.431407059342,4.20871002513732));
#2611=CARTESIAN_POINT('Ctrl Pts',(-1.22686674457499,-13.4446014654523,4.30518556038407));
#2612=CARTESIAN_POINT('Ctrl Pts',(-1.00475112921042,-13.4630160869044,4.52766249210203));
#2613=CARTESIAN_POINT('Ctrl Pts',(-0.908716991768159,-13.4695324913417,
4.66807240292884));
#2614=CARTESIAN_POINT('Ctrl Pts',(-0.78134123303562,-13.4775212102557,4.97580574542079));
#2615=CARTESIAN_POINT('Ctrl Pts',(-0.75,-13.4791505667086,5.1431252409527));
#2616=CARTESIAN_POINT('Ctrl Pts',(-0.75,-13.4791505667086,5.4568747590473));
#2617=CARTESIAN_POINT('Ctrl Pts',(-0.781341233035619,-13.4775212102557,
5.62419425457921));
#2618=CARTESIAN_POINT('Ctrl Pts',(-0.908716991768159,-13.4695324913417,
5.93192759707116));
#2619=CARTESIAN_POINT('Ctrl Pts',(-1.00475112921042,-13.4630160869044,6.07233750789797));
#2620=CARTESIAN_POINT('Ctrl Pts',(-1.22686674457499,-13.4446014654523,6.29481443961593));
#2621=CARTESIAN_POINT('Ctrl Pts',(-1.36798879559555,-13.431407059342,6.39128997486268));
#2622=CARTESIAN_POINT('Ctrl Pts',(-1.67642144832971,-13.3964062370615,6.51887197142702));
#2623=CARTESIAN_POINT('Ctrl Pts',(-1.84370531767661,-13.3744430502294,6.55));
#2624=CARTESIAN_POINT('Ctrl Pts',(-2.15801374389282,-13.3273592779611,6.55));
#2625=CARTESIAN_POINT('Ctrl Pts',(-2.32609557960331,-13.2990210880236,6.51825552186166));
#2626=CARTESIAN_POINT('Ctrl Pts',(-2.6349594886099,-13.2412866081987,6.38963814030342));
#2627=CARTESIAN_POINT('Ctrl Pts',(-2.77577516736032,-13.2120416331141,6.29277806157361));
#2628=CARTESIAN_POINT('Ctrl Pts',(-2.99640130889512,-13.163742383297,6.07057038726816));
#2629=CARTESIAN_POINT('Ctrl Pts',(-3.09176308346025,-13.1413566197491,5.93094872999216));
#2630=CARTESIAN_POINT('Ctrl Pts',(-3.21857778155664,-13.1108737267815,5.6242083709253));
#2631=CARTESIAN_POINT('Ctrl Pts',(-3.25,-13.1029576813787,5.4570590075267));
#2632=CARTESIAN_POINT('Ctrl Pts',(-3.25,-13.1029576813787,5.3));
#2633=CARTESIAN_POINT('Origin',(2.,26.9,5.3));
#2634=CARTESIAN_POINT('',(0.75,26.8,5.3));
#2635=CARTESIAN_POINT('',(0.65,26.9,5.3));
#2636=CARTESIAN_POINT('Origin',(2.,26.8,5.3));
#2637=CARTESIAN_POINT('Origin',(2.,0.,5.3));
#2638=CARTESIAN_POINT('',(0.75,13.4791505667086,5.3));
#2639=CARTESIAN_POINT('Ctrl Pts',(0.75,13.4791505667086,5.3));
#2640=CARTESIAN_POINT('Ctrl Pts',(0.75,13.4791505667086,5.4568747590473));
#2641=CARTESIAN_POINT('Ctrl Pts',(0.781341233035619,13.4775212102557,5.62419425457921));
#2642=CARTESIAN_POINT('Ctrl Pts',(0.908716991768159,13.4695324913417,5.93192759707116));
#2643=CARTESIAN_POINT('Ctrl Pts',(1.00475112921042,13.4630160869044,6.07233750789797));
#2644=CARTESIAN_POINT('Ctrl Pts',(1.22686674457499,13.4446014654523,6.29481443961593));
#2645=CARTESIAN_POINT('Ctrl Pts',(1.36798879559555,13.431407059342,6.39128997486268));
#2646=CARTESIAN_POINT('Ctrl Pts',(1.67642144832971,13.3964062370615,6.51887197142702));
#2647=CARTESIAN_POINT('Ctrl Pts',(1.84370531767661,13.3744430502294,6.55));
#2648=CARTESIAN_POINT('Ctrl Pts',(2.15801374389282,13.3273592779611,6.55));
#2649=CARTESIAN_POINT('Ctrl Pts',(2.32609557960331,13.2990210880236,6.51825552186166));
#2650=CARTESIAN_POINT('Ctrl Pts',(2.6349594886099,13.2412866081987,6.38963814030341));
#2651=CARTESIAN_POINT('Ctrl Pts',(2.77577516736032,13.2120416331141,6.29277806157361));
#2652=CARTESIAN_POINT('Ctrl Pts',(2.99640130889512,13.163742383297,6.07057038726816));
#2653=CARTESIAN_POINT('Ctrl Pts',(3.09176308346025,13.1413566197491,5.93094872999216));
#2654=CARTESIAN_POINT('Ctrl Pts',(3.21857778155664,13.1108737267815,5.6242083709253));
#2655=CARTESIAN_POINT('Ctrl Pts',(3.25,13.1029576813787,5.45705900752669));
#2656=CARTESIAN_POINT('Ctrl Pts',(3.25,13.1029576813787,5.1429409924733));
#2657=CARTESIAN_POINT('Ctrl Pts',(3.21857778155664,13.1108737267815,4.97579162907471));
#2658=CARTESIAN_POINT('Ctrl Pts',(3.09176308346025,13.1413566197491,4.66905127000784));
#2659=CARTESIAN_POINT('Ctrl Pts',(2.99640130889512,13.163742383297,4.52942961273184));
#2660=CARTESIAN_POINT('Ctrl Pts',(2.77577516736032,13.2120416331141,4.30722193842639));
#2661=CARTESIAN_POINT('Ctrl Pts',(2.6349594886099,13.2412866081987,4.21036185969658));
#2662=CARTESIAN_POINT('Ctrl Pts',(2.32609557960331,13.2990210880236,4.08174447813834));
#2663=CARTESIAN_POINT('Ctrl Pts',(2.15801374389282,13.3273592779611,4.05));
#2664=CARTESIAN_POINT('Ctrl Pts',(1.84370531767661,13.3744430502294,4.05));
#2665=CARTESIAN_POINT('Ctrl Pts',(1.67642144832972,13.3964062370615,4.08112802857298));
#2666=CARTESIAN_POINT('Ctrl Pts',(1.36798879559555,13.431407059342,4.20871002513732));
#2667=CARTESIAN_POINT('Ctrl Pts',(1.22686674457499,13.4446014654523,4.30518556038407));
#2668=CARTESIAN_POINT('Ctrl Pts',(1.00475112921042,13.4630160869044,4.52766249210203));
#2669=CARTESIAN_POINT('Ctrl Pts',(0.908716991768159,13.4695324913417,4.66807240292884));
#2670=CARTESIAN_POINT('Ctrl Pts',(0.78134123303562,13.4775212102557,4.97580574542079));
#2671=CARTESIAN_POINT('Ctrl Pts',(0.75,13.4791505667086,5.1431252409527));
#2672=CARTESIAN_POINT('Ctrl Pts',(0.75,13.4791505667086,5.3));
#2673=CARTESIAN_POINT('',(0.75,0.,5.3));
#2674=CARTESIAN_POINT('Origin',(2.,-26.9,5.3));
#2675=CARTESIAN_POINT('',(0.75,-26.8,5.3));
#2676=CARTESIAN_POINT('',(0.65,-26.9,5.3));
#2677=CARTESIAN_POINT('Origin',(2.,-26.8,5.3));
#2678=CARTESIAN_POINT('Origin',(2.,0.,5.3));
#2679=CARTESIAN_POINT('',(0.75,-13.4791505667086,5.3));
#2680=CARTESIAN_POINT('',(0.75,0.,5.3));
#2681=CARTESIAN_POINT('Ctrl Pts',(0.75,-13.4791505667086,5.3));
#2682=CARTESIAN_POINT('Ctrl Pts',(0.75,-13.4791505667086,5.1431252409527));
#2683=CARTESIAN_POINT('Ctrl Pts',(0.78134123303562,-13.4775212102557,4.97580574542079));
#2684=CARTESIAN_POINT('Ctrl Pts',(0.908716991768159,-13.4695324913417,4.66807240292884));
#2685=CARTESIAN_POINT('Ctrl Pts',(1.00475112921042,-13.4630160869044,4.52766249210203));
#2686=CARTESIAN_POINT('Ctrl Pts',(1.22686674457499,-13.4446014654523,4.30518556038407));
#2687=CARTESIAN_POINT('Ctrl Pts',(1.36798879559555,-13.431407059342,4.20871002513732));
#2688=CARTESIAN_POINT('Ctrl Pts',(1.67642144832971,-13.3964062370615,4.08112802857298));
#2689=CARTESIAN_POINT('Ctrl Pts',(1.84370531767661,-13.3744430502294,4.05));
#2690=CARTESIAN_POINT('Ctrl Pts',(2.15801374389282,-13.3273592779611,4.05));
#2691=CARTESIAN_POINT('Ctrl Pts',(2.32609557960331,-13.2990210880236,4.08174447813834));
#2692=CARTESIAN_POINT('Ctrl Pts',(2.6349594886099,-13.2412866081987,4.21036185969658));
#2693=CARTESIAN_POINT('Ctrl Pts',(2.77577516736032,-13.2120416331141,4.30722193842639));
#2694=CARTESIAN_POINT('Ctrl Pts',(2.99640130889512,-13.163742383297,4.52942961273184));
#2695=CARTESIAN_POINT('Ctrl Pts',(3.09176308346025,-13.1413566197491,4.66905127000784));
#2696=CARTESIAN_POINT('Ctrl Pts',(3.21857778155663,-13.1108737267815,4.97579162907471));
#2697=CARTESIAN_POINT('Ctrl Pts',(3.25,-13.1029576813787,5.1429409924733));
#2698=CARTESIAN_POINT('Ctrl Pts',(3.25,-13.1029576813787,5.45705900752669));
#2699=CARTESIAN_POINT('Ctrl Pts',(3.21857778155664,-13.1108737267815,5.6242083709253));
#2700=CARTESIAN_POINT('Ctrl Pts',(3.09176308346025,-13.1413566197491,5.93094872999216));
#2701=CARTESIAN_POINT('Ctrl Pts',(2.99640130889512,-13.163742383297,6.07057038726816));
#2702=CARTESIAN_POINT('Ctrl Pts',(2.77577516736032,-13.2120416331141,6.29277806157361));
#2703=CARTESIAN_POINT('Ctrl Pts',(2.6349594886099,-13.2412866081987,6.38963814030341));
#2704=CARTESIAN_POINT('Ctrl Pts',(2.32609557960331,-13.2990210880236,6.51825552186166));
#2705=CARTESIAN_POINT('Ctrl Pts',(2.15801374389282,-13.3273592779611,6.55));
#2706=CARTESIAN_POINT('Ctrl Pts',(1.84370531767661,-13.3744430502294,6.55));
#2707=CARTESIAN_POINT('Ctrl Pts',(1.67642144832971,-13.3964062370615,6.51887197142702));
#2708=CARTESIAN_POINT('Ctrl Pts',(1.36798879559555,-13.431407059342,6.39128997486268));
#2709=CARTESIAN_POINT('Ctrl Pts',(1.22686674457499,-13.4446014654523,6.29481443961593));
#2710=CARTESIAN_POINT('Ctrl Pts',(1.00475112921042,-13.4630160869044,6.07233750789797));
#2711=CARTESIAN_POINT('Ctrl Pts',(0.908716991768159,-13.4695324913417,5.93192759707116));
#2712=CARTESIAN_POINT('Ctrl Pts',(0.78134123303562,-13.4775212102557,5.62419425457921));
#2713=CARTESIAN_POINT('Ctrl Pts',(0.75,-13.4791505667086,5.4568747590473));
#2714=CARTESIAN_POINT('Ctrl Pts',(0.75,-13.4791505667086,5.3));
#2715=CARTESIAN_POINT('Origin',(0.,2.,5.3));
#2716=CARTESIAN_POINT('',(-20.2009618943233,3.25,5.3));
#2717=CARTESIAN_POINT('',(-18.627718676731,2.,6.55));
#2718=CARTESIAN_POINT('Ctrl Pts',(-20.2009618943233,3.25,5.3));
#2719=CARTESIAN_POINT('Ctrl Pts',(-20.2009618943233,3.25,5.39029234212096));
#2720=CARTESIAN_POINT('Ctrl Pts',(-20.1772005951641,3.24064153091951,5.47120219564432));
#2721=CARTESIAN_POINT('Ctrl Pts',(-20.1045047934154,3.2100076151372,5.62308391879915));
#2722=CARTESIAN_POINT('Ctrl Pts',(-20.0552828276892,3.18851767079192,5.69387466967946));
#2723=CARTESIAN_POINT('Ctrl Pts',(-19.8870287687914,3.10865620052542,5.89516586902311));
#2724=CARTESIAN_POINT('Ctrl Pts',(-19.7488255069301,3.03425420344229,6.01333284729064));
#2725=CARTESIAN_POINT('Ctrl Pts',(-19.4531336124367,2.84596078128561,6.23475573757803));
#2726=CARTESIAN_POINT('Ctrl Pts',(-19.2692763372079,2.70748360064366,6.34637446065784));
#2727=CARTESIAN_POINT('Ctrl Pts',(-18.9234249011479,2.38072616471554,6.50435864359466));
#2728=CARTESIAN_POINT('Ctrl Pts',(-18.7614575952714,2.19206789895891,6.55));
#2729=CARTESIAN_POINT('Ctrl Pts',(-18.627718676731,2.,6.55));
#2730=CARTESIAN_POINT('Ctrl Pts',(-18.627718676731,2.,6.55));
#2731=CARTESIAN_POINT('Ctrl Pts',(-18.5268891231803,1.85519457825137,6.55));
#2732=CARTESIAN_POINT('Ctrl Pts',(-18.4305104297577,1.69087323617109,6.52306381241391));
#2733=CARTESIAN_POINT('Ctrl Pts',(-18.2767214624013,1.37524312511396,6.39595782382434));
#2734=CARTESIAN_POINT('Ctrl Pts',(-18.2187291193599,1.22443201701213,6.29525819606588));
#2735=CARTESIAN_POINT('Ctrl Pts',(-18.1436817901795,0.998771663818447,6.06355058537597));
#2736=CARTESIAN_POINT('Ctrl Pts',(-18.1184989197252,0.905294021223847,5.92537474512899));
#2737=CARTESIAN_POINT('Ctrl Pts',(-18.0876253164435,0.780900542172468,5.62135879792505));
#2738=CARTESIAN_POINT('Ctrl Pts',(-18.0813014172057,0.75,5.45557706538823));
#2739=CARTESIAN_POINT('Ctrl Pts',(-18.0813014172057,0.75,5.14442293461177));
#2740=CARTESIAN_POINT('Ctrl Pts',(-18.0876253164435,0.780900542172469,4.97864120207495));
#2741=CARTESIAN_POINT('Ctrl Pts',(-18.1184989197252,0.905294021223848,4.67462525487101));
#2742=CARTESIAN_POINT('Ctrl Pts',(-18.1436817901795,0.998771663818447,4.53644941462403));
#2743=CARTESIAN_POINT('Ctrl Pts',(-18.2187291193599,1.22443201701213,4.30474180393412));
#2744=CARTESIAN_POINT('Ctrl Pts',(-18.2767214624013,1.37524312511396,4.20404217617566));
#2745=CARTESIAN_POINT('Ctrl Pts',(-18.4305104297577,1.69087323617109,4.07693618758609));
#2746=CARTESIAN_POINT('Ctrl Pts',(-18.5268891231803,1.85519457825137,4.05));
#2747=CARTESIAN_POINT('Ctrl Pts',(-18.7614575952714,2.19206789895891,4.05));
#2748=CARTESIAN_POINT('Ctrl Pts',(-18.9234249011479,2.38072616471554,4.09564135640534));
#2749=CARTESIAN_POINT('Ctrl Pts',(-19.2692763372079,2.70748360064366,4.25362553934216));
#2750=CARTESIAN_POINT('Ctrl Pts',(-19.4531336124367,2.84596078128562,4.36524426242197));
#2751=CARTESIAN_POINT('Ctrl Pts',(-19.7488255069301,3.03425420344229,4.58666715270936));
#2752=CARTESIAN_POINT('Ctrl Pts',(-19.8870287687914,3.10865620052542,4.70483413097689));
#2753=CARTESIAN_POINT('Ctrl Pts',(-20.0552828276892,3.18851767079192,4.90612533032054));
#2754=CARTESIAN_POINT('Ctrl Pts',(-20.1045047934154,3.2100076151372,4.97691608120085));
#2755=CARTESIAN_POINT('Ctrl Pts',(-20.1772005951641,3.24064153091951,5.12879780435568));
#2756=CARTESIAN_POINT('Ctrl Pts',(-20.2009618943233,3.25,5.20970765787903));
#2757=CARTESIAN_POINT('Ctrl Pts',(-20.2009618943233,3.25,5.3));
#2758=CARTESIAN_POINT('',(-13.3510299228187,2.,6.55));
#2759=CARTESIAN_POINT('',(0.,2.,6.55));
#2760=CARTESIAN_POINT('',(-13.1029576813787,3.25,5.3));
#2761=CARTESIAN_POINT('Ctrl Pts',(-13.1029576813787,3.25,5.3));
#2762=CARTESIAN_POINT('Ctrl Pts',(-13.1029576813787,3.25,5.1429409924733));
#2763=CARTESIAN_POINT('Ctrl Pts',(-13.1108737267815,3.21857778155663,4.97579162907471));
#2764=CARTESIAN_POINT('Ctrl Pts',(-13.1413566197491,3.09176308346025,4.66905127000784));
#2765=CARTESIAN_POINT('Ctrl Pts',(-13.163742383297,2.99640130889512,4.52942961273184));
#2766=CARTESIAN_POINT('Ctrl Pts',(-13.2120416331141,2.77577516736032,4.30722193842639));
#2767=CARTESIAN_POINT('Ctrl Pts',(-13.2412866081987,2.6349594886099,4.21036185969658));
#2768=CARTESIAN_POINT('Ctrl Pts',(-13.2990210880236,2.32609557960331,4.08174447813834));
#2769=CARTESIAN_POINT('Ctrl Pts',(-13.3273592779611,2.15801374389282,4.05));
#2770=CARTESIAN_POINT('Ctrl Pts',(-13.3744430502294,1.84370531767661,4.05));
#2771=CARTESIAN_POINT('Ctrl Pts',(-13.3964062370615,1.67642144832971,4.08112802857298));
#2772=CARTESIAN_POINT('Ctrl Pts',(-13.431407059342,1.36798879559555,4.20871002513732));
#2773=CARTESIAN_POINT('Ctrl Pts',(-13.4446014654523,1.22686674457499,4.30518556038407));
#2774=CARTESIAN_POINT('Ctrl Pts',(-13.4630160869044,1.00475112921042,4.52766249210203));
#2775=CARTESIAN_POINT('Ctrl Pts',(-13.4695324913417,0.908716991768159,4.66807240292884));
#2776=CARTESIAN_POINT('Ctrl Pts',(-13.4775212102557,0.78134123303562,4.97580574542079));
#2777=CARTESIAN_POINT('Ctrl Pts',(-13.4791505667086,0.75,5.1431252409527));
#2778=CARTESIAN_POINT('Ctrl Pts',(-13.4791505667086,0.75,5.4568747590473));
#2779=CARTESIAN_POINT('Ctrl Pts',(-13.4775212102557,0.781341233035619,5.62419425457921));
#2780=CARTESIAN_POINT('Ctrl Pts',(-13.4695324913417,0.908716991768159,5.93192759707116));
#2781=CARTESIAN_POINT('Ctrl Pts',(-13.4630160869044,1.00475112921042,6.07233750789797));
#2782=CARTESIAN_POINT('Ctrl Pts',(-13.4446014654523,1.22686674457499,6.29481443961593));
#2783=CARTESIAN_POINT('Ctrl Pts',(-13.431407059342,1.36798879559555,6.39128997486268));
#2784=CARTESIAN_POINT('Ctrl Pts',(-13.3964062370615,1.67642144832971,6.51887197142702));
#2785=CARTESIAN_POINT('Ctrl Pts',(-13.3744430502294,1.84370531767661,6.55));
#2786=CARTESIAN_POINT('Ctrl Pts',(-13.3510299228187,2.,6.55));
#2787=CARTESIAN_POINT('Ctrl Pts',(-13.3510299228187,2.,6.55));
#2788=CARTESIAN_POINT('Ctrl Pts',(-13.3273592779611,2.15801374389282,6.55));
#2789=CARTESIAN_POINT('Ctrl Pts',(-13.2990210880236,2.32609557960331,6.51825552186166));
#2790=CARTESIAN_POINT('Ctrl Pts',(-13.2412866081987,2.6349594886099,6.38963814030342));
#2791=CARTESIAN_POINT('Ctrl Pts',(-13.2120416331141,2.77577516736032,6.29277806157361));
#2792=CARTESIAN_POINT('Ctrl Pts',(-13.163742383297,2.99640130889512,6.07057038726816));
#2793=CARTESIAN_POINT('Ctrl Pts',(-13.1413566197491,3.09176308346025,5.93094872999216));
#2794=CARTESIAN_POINT('Ctrl Pts',(-13.1108737267815,3.21857778155664,5.6242083709253));
#2795=CARTESIAN_POINT('Ctrl Pts',(-13.1029576813787,3.25,5.4570590075267));
#2796=CARTESIAN_POINT('Ctrl Pts',(-13.1029576813787,3.25,5.3));
#2797=CARTESIAN_POINT('Origin',(0.,2.,5.3));
#2798=CARTESIAN_POINT('',(13.1029576813787,3.25,5.3));
#2799=CARTESIAN_POINT('',(13.3510299228187,2.,6.55));
#2800=CARTESIAN_POINT('Ctrl Pts',(13.1029576813787,3.25,5.3));
#2801=CARTESIAN_POINT('Ctrl Pts',(13.1029576813787,3.25,5.45705900752669));
#2802=CARTESIAN_POINT('Ctrl Pts',(13.1108737267815,3.21857778155664,5.6242083709253));
#2803=CARTESIAN_POINT('Ctrl Pts',(13.1413566197491,3.09176308346025,5.93094872999216));
#2804=CARTESIAN_POINT('Ctrl Pts',(13.163742383297,2.99640130889512,6.07057038726816));
#2805=CARTESIAN_POINT('Ctrl Pts',(13.2120416331141,2.77577516736032,6.29277806157361));
#2806=CARTESIAN_POINT('Ctrl Pts',(13.2412866081987,2.6349594886099,6.38963814030342));
#2807=CARTESIAN_POINT('Ctrl Pts',(13.2990210880236,2.32609557960331,6.51825552186166));
#2808=CARTESIAN_POINT('Ctrl Pts',(13.3273592779611,2.15801374389282,6.55));
#2809=CARTESIAN_POINT('Ctrl Pts',(13.3510299228187,2.,6.55));
#2810=CARTESIAN_POINT('Ctrl Pts',(13.3510299228187,2.,6.55));
#2811=CARTESIAN_POINT('Ctrl Pts',(13.3744430502294,1.84370531767661,6.55));
#2812=CARTESIAN_POINT('Ctrl Pts',(13.3964062370615,1.67642144832971,6.51887197142702));
#2813=CARTESIAN_POINT('Ctrl Pts',(13.431407059342,1.36798879559555,6.39128997486268));
#2814=CARTESIAN_POINT('Ctrl Pts',(13.4446014654523,1.22686674457499,6.29481443961593));
#2815=CARTESIAN_POINT('Ctrl Pts',(13.4630160869044,1.00475112921042,6.07233750789797));
#2816=CARTESIAN_POINT('Ctrl Pts',(13.4695324913417,0.908716991768159,5.93192759707116));
#2817=CARTESIAN_POINT('Ctrl Pts',(13.4775212102557,0.781341233035619,5.62419425457921));
#2818=CARTESIAN_POINT('Ctrl Pts',(13.4791505667086,0.75,5.4568747590473));
#2819=CARTESIAN_POINT('Ctrl Pts',(13.4791505667086,0.75,5.1431252409527));
#2820=CARTESIAN_POINT('Ctrl Pts',(13.4775212102557,0.78134123303562,4.97580574542079));
#2821=CARTESIAN_POINT('Ctrl Pts',(13.4695324913417,0.908716991768159,4.66807240292884));
#2822=CARTESIAN_POINT('Ctrl Pts',(13.4630160869044,1.00475112921042,4.52766249210203));
#2823=CARTESIAN_POINT('Ctrl Pts',(13.4446014654523,1.22686674457499,4.30518556038407));
#2824=CARTESIAN_POINT('Ctrl Pts',(13.431407059342,1.36798879559555,4.20871002513732));
#2825=CARTESIAN_POINT('Ctrl Pts',(13.3964062370615,1.67642144832971,4.08112802857298));
#2826=CARTESIAN_POINT('Ctrl Pts',(13.3744430502294,1.84370531767661,4.05));
#2827=CARTESIAN_POINT('Ctrl Pts',(13.3273592779611,2.15801374389282,4.05));
#2828=CARTESIAN_POINT('Ctrl Pts',(13.2990210880236,2.32609557960331,4.08174447813834));
#2829=CARTESIAN_POINT('Ctrl Pts',(13.2412866081987,2.6349594886099,4.21036185969658));
#2830=CARTESIAN_POINT('Ctrl Pts',(13.2120416331141,2.77577516736032,4.30722193842639));
#2831=CARTESIAN_POINT('Ctrl Pts',(13.163742383297,2.99640130889512,4.52942961273184));
#2832=CARTESIAN_POINT('Ctrl Pts',(13.1413566197491,3.09176308346025,4.66905127000784));
#2833=CARTESIAN_POINT('Ctrl Pts',(13.1108737267815,3.21857778155663,4.97579162907471));
#2834=CARTESIAN_POINT('Ctrl Pts',(13.1029576813787,3.25,5.1429409924733));
#2835=CARTESIAN_POINT('Ctrl Pts',(13.1029576813787,3.25,5.3));
#2836=CARTESIAN_POINT('',(18.627718676731,2.,6.55));
#2837=CARTESIAN_POINT('',(0.,2.,6.55));
#2838=CARTESIAN_POINT('',(20.2009618943233,3.25,5.3));
#2839=CARTESIAN_POINT('Ctrl Pts',(20.2009618943233,3.25,5.3));
#2840=CARTESIAN_POINT('Ctrl Pts',(20.2009618943233,3.25,5.20970765787903));
#2841=CARTESIAN_POINT('Ctrl Pts',(20.1772005951641,3.24064153091951,5.12879780435568));
#2842=CARTESIAN_POINT('Ctrl Pts',(20.1045047934154,3.2100076151372,4.97691608120085));
#2843=CARTESIAN_POINT('Ctrl Pts',(20.0552828276892,3.18851767079192,4.90612533032054));
#2844=CARTESIAN_POINT('Ctrl Pts',(19.8870287687914,3.10865620052542,4.70483413097689));
#2845=CARTESIAN_POINT('Ctrl Pts',(19.7488255069301,3.03425420344229,4.58666715270936));
#2846=CARTESIAN_POINT('Ctrl Pts',(19.4531336124367,2.84596078128561,4.36524426242197));
#2847=CARTESIAN_POINT('Ctrl Pts',(19.2692763372079,2.70748360064366,4.25362553934216));
#2848=CARTESIAN_POINT('Ctrl Pts',(18.9234249011479,2.38072616471554,4.09564135640534));
#2849=CARTESIAN_POINT('Ctrl Pts',(18.7614575952714,2.19206789895891,4.05));
#2850=CARTESIAN_POINT('Ctrl Pts',(18.5268891231803,1.85519457825137,4.05));
#2851=CARTESIAN_POINT('Ctrl Pts',(18.4305104297577,1.69087323617109,4.07693618758609));
#2852=CARTESIAN_POINT('Ctrl Pts',(18.2767214624013,1.37524312511396,4.20404217617566));
#2853=CARTESIAN_POINT('Ctrl Pts',(18.2187291193599,1.22443201701213,4.30474180393412));
#2854=CARTESIAN_POINT('Ctrl Pts',(18.1436817901795,0.998771663818447,4.53644941462403));
#2855=CARTESIAN_POINT('Ctrl Pts',(18.1184989197252,0.905294021223847,4.67462525487101));
#2856=CARTESIAN_POINT('Ctrl Pts',(18.0876253164435,0.780900542172469,4.97864120207495));
#2857=CARTESIAN_POINT('Ctrl Pts',(18.0813014172057,0.75,5.14442293461177));
#2858=CARTESIAN_POINT('Ctrl Pts',(18.0813014172057,0.75,5.45557706538823));
#2859=CARTESIAN_POINT('Ctrl Pts',(18.0876253164435,0.780900542172469,5.62135879792505));
#2860=CARTESIAN_POINT('Ctrl Pts',(18.1184989197252,0.905294021223848,5.92537474512899));
#2861=CARTESIAN_POINT('Ctrl Pts',(18.1436817901795,0.998771663818447,6.06355058537597));
#2862=CARTESIAN_POINT('Ctrl Pts',(18.2187291193599,1.22443201701213,6.29525819606588));
#2863=CARTESIAN_POINT('Ctrl Pts',(18.2767214624013,1.37524312511396,6.39595782382434));
#2864=CARTESIAN_POINT('Ctrl Pts',(18.4305104297577,1.69087323617109,6.52306381241391));
#2865=CARTESIAN_POINT('Ctrl Pts',(18.5268891231803,1.85519457825137,6.55));
#2866=CARTESIAN_POINT('Ctrl Pts',(18.627718676731,2.,6.55));
#2867=CARTESIAN_POINT('Ctrl Pts',(18.627718676731,2.,6.55));
#2868=CARTESIAN_POINT('Ctrl Pts',(18.7614575952714,2.19206789895891,6.55));
#2869=CARTESIAN_POINT('Ctrl Pts',(18.9234249011479,2.38072616471554,6.50435864359466));
#2870=CARTESIAN_POINT('Ctrl Pts',(19.2692763372079,2.70748360064366,6.34637446065784));
#2871=CARTESIAN_POINT('Ctrl Pts',(19.4531336124367,2.84596078128561,6.23475573757803));
#2872=CARTESIAN_POINT('Ctrl Pts',(19.7488255069301,3.03425420344229,6.01333284729064));
#2873=CARTESIAN_POINT('Ctrl Pts',(19.8870287687914,3.10865620052542,5.89516586902311));
#2874=CARTESIAN_POINT('Ctrl Pts',(20.0552828276892,3.18851767079192,5.69387466967946));
#2875=CARTESIAN_POINT('Ctrl Pts',(20.1045047934154,3.2100076151372,5.62308391879915));
#2876=CARTESIAN_POINT('Ctrl Pts',(20.1772005951641,3.24064153091951,5.47120219564432));
#2877=CARTESIAN_POINT('Ctrl Pts',(20.2009618943233,3.25,5.39029234212096));
#2878=CARTESIAN_POINT('Ctrl Pts',(20.2009618943233,3.25,5.3));
#2879=CARTESIAN_POINT('Origin',(0.,-2.,5.3));
#2880=CARTESIAN_POINT('',(-18.0813014172057,-0.75,5.3));
#2881=CARTESIAN_POINT('',(-18.627718676731,-2.,6.55));
#2882=CARTESIAN_POINT('Ctrl Pts',(-18.0813014172057,-0.75,5.3));
#2883=CARTESIAN_POINT('Ctrl Pts',(-18.0813014172057,-0.75,5.45557706538823));
#2884=CARTESIAN_POINT('Ctrl Pts',(-18.0876253164435,-0.780900542172469,
5.62135879792505));
#2885=CARTESIAN_POINT('Ctrl Pts',(-18.1184989197252,-0.905294021223848,
5.92537474512899));
#2886=CARTESIAN_POINT('Ctrl Pts',(-18.1436817901795,-0.998771663818447,
6.06355058537597));
#2887=CARTESIAN_POINT('Ctrl Pts',(-18.2187291193599,-1.22443201701213,6.29525819606588));
#2888=CARTESIAN_POINT('Ctrl Pts',(-18.2767214624013,-1.37524312511396,6.39595782382434));
#2889=CARTESIAN_POINT('Ctrl Pts',(-18.4305104297577,-1.69087323617109,6.52306381241391));
#2890=CARTESIAN_POINT('Ctrl Pts',(-18.5268891231803,-1.85519457825137,6.55));
#2891=CARTESIAN_POINT('Ctrl Pts',(-18.627718676731,-2.,6.55));
#2892=CARTESIAN_POINT('Ctrl Pts',(-18.627718676731,-2.,6.55));
#2893=CARTESIAN_POINT('Ctrl Pts',(-18.7614575952714,-2.19206789895891,6.55));
#2894=CARTESIAN_POINT('Ctrl Pts',(-18.9234249011479,-2.38072616471554,6.50435864359466));
#2895=CARTESIAN_POINT('Ctrl Pts',(-19.2692763372079,-2.70748360064366,6.34637446065784));
#2896=CARTESIAN_POINT('Ctrl Pts',(-19.4531336124367,-2.84596078128561,6.23475573757803));
#2897=CARTESIAN_POINT('Ctrl Pts',(-19.7488255069301,-3.03425420344229,6.01333284729064));
#2898=CARTESIAN_POINT('Ctrl Pts',(-19.8870287687914,-3.10865620052542,5.89516586902311));
#2899=CARTESIAN_POINT('Ctrl Pts',(-20.0552828276892,-3.18851767079192,5.69387466967946));
#2900=CARTESIAN_POINT('Ctrl Pts',(-20.1045047934154,-3.2100076151372,5.62308391879915));
#2901=CARTESIAN_POINT('Ctrl Pts',(-20.1772005951641,-3.24064153091951,5.47120219564432));
#2902=CARTESIAN_POINT('Ctrl Pts',(-20.2009618943233,-3.25,5.39029234212096));
#2903=CARTESIAN_POINT('Ctrl Pts',(-20.2009618943233,-3.25,5.20970765787903));
#2904=CARTESIAN_POINT('Ctrl Pts',(-20.1772005951641,-3.24064153091951,5.12879780435568));
#2905=CARTESIAN_POINT('Ctrl Pts',(-20.1045047934154,-3.2100076151372,4.97691608120085));
#2906=CARTESIAN_POINT('Ctrl Pts',(-20.0552828276892,-3.18851767079192,4.90612533032054));
#2907=CARTESIAN_POINT('Ctrl Pts',(-19.8870287687914,-3.10865620052542,4.70483413097689));
#2908=CARTESIAN_POINT('Ctrl Pts',(-19.7488255069301,-3.03425420344229,4.58666715270936));
#2909=CARTESIAN_POINT('Ctrl Pts',(-19.4531336124367,-2.84596078128561,4.36524426242197));
#2910=CARTESIAN_POINT('Ctrl Pts',(-19.2692763372079,-2.70748360064366,4.25362553934216));
#2911=CARTESIAN_POINT('Ctrl Pts',(-18.9234249011479,-2.38072616471554,4.09564135640534));
#2912=CARTESIAN_POINT('Ctrl Pts',(-18.7614575952714,-2.19206789895891,4.05));
#2913=CARTESIAN_POINT('Ctrl Pts',(-18.5268891231803,-1.85519457825137,4.05));
#2914=CARTESIAN_POINT('Ctrl Pts',(-18.4305104297577,-1.69087323617109,4.0769361875861));
#2915=CARTESIAN_POINT('Ctrl Pts',(-18.2767214624013,-1.37524312511396,4.20404217617566));
#2916=CARTESIAN_POINT('Ctrl Pts',(-18.2187291193599,-1.22443201701213,4.30474180393412));
#2917=CARTESIAN_POINT('Ctrl Pts',(-18.1436817901795,-0.998771663818447,
4.53644941462403));
#2918=CARTESIAN_POINT('Ctrl Pts',(-18.1184989197252,-0.905294021223848,
4.67462525487101));
#2919=CARTESIAN_POINT('Ctrl Pts',(-18.0876253164435,-0.780900542172469,
4.97864120207495));
#2920=CARTESIAN_POINT('Ctrl Pts',(-18.0813014172057,-0.75,5.14442293461177));
#2921=CARTESIAN_POINT('Ctrl Pts',(-18.0813014172057,-0.75,5.3));
#2922=CARTESIAN_POINT('',(-13.3510299228187,-2.,6.55));
#2923=CARTESIAN_POINT('',(0.,-2.,6.55));
#2924=CARTESIAN_POINT('',(-13.4791505667086,-0.75,5.3));
#2925=CARTESIAN_POINT('Ctrl Pts',(-13.4791505667086,-0.75,5.3));
#2926=CARTESIAN_POINT('Ctrl Pts',(-13.4791505667086,-0.75,5.1431252409527));
#2927=CARTESIAN_POINT('Ctrl Pts',(-13.4775212102557,-0.78134123303562,4.97580574542079));
#2928=CARTESIAN_POINT('Ctrl Pts',(-13.4695324913417,-0.908716991768159,
4.66807240292884));
#2929=CARTESIAN_POINT('Ctrl Pts',(-13.4630160869044,-1.00475112921042,4.52766249210203));
#2930=CARTESIAN_POINT('Ctrl Pts',(-13.4446014654523,-1.22686674457499,4.30518556038407));
#2931=CARTESIAN_POINT('Ctrl Pts',(-13.431407059342,-1.36798879559555,4.20871002513732));
#2932=CARTESIAN_POINT('Ctrl Pts',(-13.3964062370615,-1.67642144832972,4.08112802857298));
#2933=CARTESIAN_POINT('Ctrl Pts',(-13.3744430502294,-1.84370531767661,4.05));
#2934=CARTESIAN_POINT('Ctrl Pts',(-13.3273592779611,-2.15801374389282,4.05));
#2935=CARTESIAN_POINT('Ctrl Pts',(-13.2990210880236,-2.32609557960331,4.08174447813834));
#2936=CARTESIAN_POINT('Ctrl Pts',(-13.2412866081987,-2.6349594886099,4.21036185969658));
#2937=CARTESIAN_POINT('Ctrl Pts',(-13.2120416331141,-2.77577516736032,4.30722193842639));
#2938=CARTESIAN_POINT('Ctrl Pts',(-13.163742383297,-2.99640130889512,4.52942961273184));
#2939=CARTESIAN_POINT('Ctrl Pts',(-13.1413566197491,-3.09176308346025,4.66905127000784));
#2940=CARTESIAN_POINT('Ctrl Pts',(-13.1108737267815,-3.21857778155663,4.97579162907471));
#2941=CARTESIAN_POINT('Ctrl Pts',(-13.1029576813787,-3.25,5.1429409924733));
#2942=CARTESIAN_POINT('Ctrl Pts',(-13.1029576813787,-3.25,5.45705900752669));
#2943=CARTESIAN_POINT('Ctrl Pts',(-13.1108737267815,-3.21857778155664,5.6242083709253));
#2944=CARTESIAN_POINT('Ctrl Pts',(-13.1413566197491,-3.09176308346025,5.93094872999216));
#2945=CARTESIAN_POINT('Ctrl Pts',(-13.163742383297,-2.99640130889512,6.07057038726816));
#2946=CARTESIAN_POINT('Ctrl Pts',(-13.2120416331141,-2.77577516736032,6.29277806157361));
#2947=CARTESIAN_POINT('Ctrl Pts',(-13.2412866081987,-2.6349594886099,6.38963814030341));
#2948=CARTESIAN_POINT('Ctrl Pts',(-13.2990210880236,-2.32609557960331,6.51825552186166));
#2949=CARTESIAN_POINT('Ctrl Pts',(-13.3273592779611,-2.15801374389282,6.55));
#2950=CARTESIAN_POINT('Ctrl Pts',(-13.3510299228187,-2.,6.55));
#2951=CARTESIAN_POINT('Ctrl Pts',(-13.3510299228187,-2.,6.55));
#2952=CARTESIAN_POINT('Ctrl Pts',(-13.3744430502294,-1.84370531767661,6.55));
#2953=CARTESIAN_POINT('Ctrl Pts',(-13.3964062370615,-1.67642144832971,6.51887197142702));
#2954=CARTESIAN_POINT('Ctrl Pts',(-13.431407059342,-1.36798879559555,6.39128997486268));
#2955=CARTESIAN_POINT('Ctrl Pts',(-13.4446014654523,-1.22686674457499,6.29481443961593));
#2956=CARTESIAN_POINT('Ctrl Pts',(-13.4630160869044,-1.00475112921042,6.07233750789797));
#2957=CARTESIAN_POINT('Ctrl Pts',(-13.4695324913417,-0.908716991768159,
5.93192759707116));
#2958=CARTESIAN_POINT('Ctrl Pts',(-13.4775212102557,-0.781341233035619,
5.62419425457921));
#2959=CARTESIAN_POINT('Ctrl Pts',(-13.4791505667086,-0.75,5.4568747590473));
#2960=CARTESIAN_POINT('Ctrl Pts',(-13.4791505667086,-0.75,5.3));
#2961=CARTESIAN_POINT('Origin',(0.,-2.,5.3));
#2962=CARTESIAN_POINT('',(13.4791505667086,-0.75,5.3));
#2963=CARTESIAN_POINT('',(13.3510299228187,-2.,6.55));
#2964=CARTESIAN_POINT('Ctrl Pts',(13.4791505667086,-0.75,5.3));
#2965=CARTESIAN_POINT('Ctrl Pts',(13.4791505667086,-0.75,5.4568747590473));
#2966=CARTESIAN_POINT('Ctrl Pts',(13.4775212102557,-0.781341233035619,5.62419425457921));
#2967=CARTESIAN_POINT('Ctrl Pts',(13.4695324913417,-0.908716991768159,5.93192759707116));
#2968=CARTESIAN_POINT('Ctrl Pts',(13.4630160869044,-1.00475112921042,6.07233750789797));
#2969=CARTESIAN_POINT('Ctrl Pts',(13.4446014654523,-1.22686674457499,6.29481443961593));
#2970=CARTESIAN_POINT('Ctrl Pts',(13.431407059342,-1.36798879559555,6.39128997486268));
#2971=CARTESIAN_POINT('Ctrl Pts',(13.3964062370615,-1.67642144832971,6.51887197142702));
#2972=CARTESIAN_POINT('Ctrl Pts',(13.3744430502294,-1.84370531767661,6.55));
#2973=CARTESIAN_POINT('Ctrl Pts',(13.3510299228187,-2.,6.55));
#2974=CARTESIAN_POINT('Ctrl Pts',(13.3510299228187,-2.,6.55));
#2975=CARTESIAN_POINT('Ctrl Pts',(13.3273592779611,-2.15801374389282,6.55));
#2976=CARTESIAN_POINT('Ctrl Pts',(13.2990210880236,-2.32609557960331,6.51825552186166));
#2977=CARTESIAN_POINT('Ctrl Pts',(13.2412866081987,-2.6349594886099,6.38963814030341));
#2978=CARTESIAN_POINT('Ctrl Pts',(13.2120416331141,-2.77577516736032,6.29277806157361));
#2979=CARTESIAN_POINT('Ctrl Pts',(13.163742383297,-2.99640130889512,6.07057038726816));
#2980=CARTESIAN_POINT('Ctrl Pts',(13.1413566197491,-3.09176308346025,5.93094872999216));
#2981=CARTESIAN_POINT('Ctrl Pts',(13.1108737267815,-3.21857778155664,5.6242083709253));
#2982=CARTESIAN_POINT('Ctrl Pts',(13.1029576813787,-3.25,5.45705900752669));
#2983=CARTESIAN_POINT('Ctrl Pts',(13.1029576813787,-3.25,5.1429409924733));
#2984=CARTESIAN_POINT('Ctrl Pts',(13.1108737267815,-3.21857778155663,4.97579162907471));
#2985=CARTESIAN_POINT('Ctrl Pts',(13.1413566197491,-3.09176308346025,4.66905127000784));
#2986=CARTESIAN_POINT('Ctrl Pts',(13.163742383297,-2.99640130889512,4.52942961273184));
#2987=CARTESIAN_POINT('Ctrl Pts',(13.2120416331141,-2.77577516736032,4.30722193842639));
#2988=CARTESIAN_POINT('Ctrl Pts',(13.2412866081987,-2.6349594886099,4.21036185969659));
#2989=CARTESIAN_POINT('Ctrl Pts',(13.2990210880236,-2.32609557960331,4.08174447813834));
#2990=CARTESIAN_POINT('Ctrl Pts',(13.3273592779611,-2.15801374389282,4.05));
#2991=CARTESIAN_POINT('Ctrl Pts',(13.3744430502294,-1.84370531767661,4.05));
#2992=CARTESIAN_POINT('Ctrl Pts',(13.3964062370615,-1.67642144832971,4.08112802857298));
#2993=CARTESIAN_POINT('Ctrl Pts',(13.431407059342,-1.36798879559555,4.20871002513732));
#2994=CARTESIAN_POINT('Ctrl Pts',(13.4446014654523,-1.22686674457499,4.30518556038407));
#2995=CARTESIAN_POINT('Ctrl Pts',(13.4630160869044,-1.00475112921042,4.52766249210203));
#2996=CARTESIAN_POINT('Ctrl Pts',(13.4695324913417,-0.908716991768158,4.66807240292885));
#2997=CARTESIAN_POINT('Ctrl Pts',(13.4775212102557,-0.781341233035619,4.97580574542079));
#2998=CARTESIAN_POINT('Ctrl Pts',(13.4791505667086,-0.75,5.1431252409527));
#2999=CARTESIAN_POINT('Ctrl Pts',(13.4791505667086,-0.75,5.3));
#3000=CARTESIAN_POINT('',(18.627718676731,-2.,6.55));
#3001=CARTESIAN_POINT('',(0.,-2.,6.55));
#3002=CARTESIAN_POINT('',(18.0813014172057,-0.75,5.3));
#3003=CARTESIAN_POINT('Ctrl Pts',(18.0813014172057,-0.75,5.3));
#3004=CARTESIAN_POINT('Ctrl Pts',(18.0813014172057,-0.75,5.14442293461177));
#3005=CARTESIAN_POINT('Ctrl Pts',(18.0876253164435,-0.780900542172469,4.97864120207495));
#3006=CARTESIAN_POINT('Ctrl Pts',(18.1184989197252,-0.905294021223848,4.67462525487101));
#3007=CARTESIAN_POINT('Ctrl Pts',(18.1436817901795,-0.998771663818447,4.53644941462403));
#3008=CARTESIAN_POINT('Ctrl Pts',(18.2187291193599,-1.22443201701213,4.30474180393412));
#3009=CARTESIAN_POINT('Ctrl Pts',(18.2767214624013,-1.37524312511396,4.20404217617566));
#3010=CARTESIAN_POINT('Ctrl Pts',(18.4305104297577,-1.69087323617109,4.07693618758609));
#3011=CARTESIAN_POINT('Ctrl Pts',(18.5268891231803,-1.85519457825137,4.05));
#3012=CARTESIAN_POINT('Ctrl Pts',(18.7614575952714,-2.19206789895891,4.05));
#3013=CARTESIAN_POINT('Ctrl Pts',(18.9234249011479,-2.38072616471554,4.09564135640534));
#3014=CARTESIAN_POINT('Ctrl Pts',(19.2692763372079,-2.70748360064366,4.25362553934216));
#3015=CARTESIAN_POINT('Ctrl Pts',(19.4531336124367,-2.84596078128561,4.36524426242197));
#3016=CARTESIAN_POINT('Ctrl Pts',(19.7488255069301,-3.03425420344229,4.58666715270936));
#3017=CARTESIAN_POINT('Ctrl Pts',(19.8870287687914,-3.10865620052542,4.70483413097689));
#3018=CARTESIAN_POINT('Ctrl Pts',(20.0552828276892,-3.18851767079192,4.90612533032054));
#3019=CARTESIAN_POINT('Ctrl Pts',(20.1045047934154,-3.2100076151372,4.97691608120085));
#3020=CARTESIAN_POINT('Ctrl Pts',(20.1772005951641,-3.24064153091951,5.12879780435568));
#3021=CARTESIAN_POINT('Ctrl Pts',(20.2009618943233,-3.25,5.20970765787903));
#3022=CARTESIAN_POINT('Ctrl Pts',(20.2009618943233,-3.25,5.39029234212096));
#3023=CARTESIAN_POINT('Ctrl Pts',(20.1772005951641,-3.24064153091951,5.47120219564432));
#3024=CARTESIAN_POINT('Ctrl Pts',(20.1045047934154,-3.2100076151372,5.62308391879915));
#3025=CARTESIAN_POINT('Ctrl Pts',(20.0552828276892,-3.18851767079192,5.69387466967946));
#3026=CARTESIAN_POINT('Ctrl Pts',(19.8870287687914,-3.10865620052542,5.89516586902311));
#3027=CARTESIAN_POINT('Ctrl Pts',(19.7488255069301,-3.03425420344229,6.01333284729064));
#3028=CARTESIAN_POINT('Ctrl Pts',(19.4531336124367,-2.84596078128561,6.23475573757803));
#3029=CARTESIAN_POINT('Ctrl Pts',(19.2692763372079,-2.70748360064366,6.34637446065784));
#3030=CARTESIAN_POINT('Ctrl Pts',(18.9234249011479,-2.38072616471554,6.50435864359466));
#3031=CARTESIAN_POINT('Ctrl Pts',(18.7614575952714,-2.19206789895891,6.55));
#3032=CARTESIAN_POINT('Ctrl Pts',(18.627718676731,-2.,6.55));
#3033=CARTESIAN_POINT('Ctrl Pts',(18.627718676731,-2.,6.55));
#3034=CARTESIAN_POINT('Ctrl Pts',(18.5268891231803,-1.85519457825137,6.55));
#3035=CARTESIAN_POINT('Ctrl Pts',(18.4305104297577,-1.69087323617109,6.52306381241391));
#3036=CARTESIAN_POINT('Ctrl Pts',(18.2767214624013,-1.37524312511396,6.39595782382434));
#3037=CARTESIAN_POINT('Ctrl Pts',(18.2187291193599,-1.22443201701213,6.29525819606588));
#3038=CARTESIAN_POINT('Ctrl Pts',(18.1436817901795,-0.998771663818447,6.06355058537597));
#3039=CARTESIAN_POINT('Ctrl Pts',(18.1184989197252,-0.905294021223848,5.92537474512899));
#3040=CARTESIAN_POINT('Ctrl Pts',(18.0876253164435,-0.780900542172469,5.62135879792505));
#3041=CARTESIAN_POINT('Ctrl Pts',(18.0813014172057,-0.75,5.45557706538823));
#3042=CARTESIAN_POINT('Ctrl Pts',(18.0813014172057,-0.75,5.3));
#3043=CARTESIAN_POINT('Origin',(21.5,0.,3.7));
#3044=CARTESIAN_POINT('',(21.5,-3.5,3.7));
#3045=CARTESIAN_POINT('Origin',(21.5,0.,3.7));
#3046=CARTESIAN_POINT('',(21.5,-3.5,9.));
#3047=CARTESIAN_POINT('',(21.5,-3.5,3.7));
#3048=CARTESIAN_POINT('Origin',(21.5,0.,9.));
#3049=CARTESIAN_POINT('Origin',(21.5,0.,3.7));
#3050=CARTESIAN_POINT('Origin',(-21.5,0.,3.7));
#3051=CARTESIAN_POINT('',(-21.5,-3.5,3.7));
#3052=CARTESIAN_POINT('Origin',(-21.5,0.,3.7));
#3053=CARTESIAN_POINT('',(-21.5,-3.5,9.));
#3054=CARTESIAN_POINT('',(-21.5,-3.5,3.7));
#3055=CARTESIAN_POINT('Origin',(-21.5,0.,9.));
#3056=CARTESIAN_POINT('Origin',(-21.5,0.,3.7));
#3057=CARTESIAN_POINT('Origin',(0.,20.3,6.9));
#3058=CARTESIAN_POINT('',(-5.025,20.3,6.9));
#3059=CARTESIAN_POINT('Origin',(0.,20.3,6.9));
#3060=CARTESIAN_POINT('',(-5.025,20.3,9.));
#3061=CARTESIAN_POINT('',(-5.025,20.3,6.9));
#3062=CARTESIAN_POINT('Origin',(0.,20.3,9.));
#3063=CARTESIAN_POINT('Origin',(0.,20.3,6.9));
#3064=CARTESIAN_POINT('Origin',(0.,-20.3,6.9));
#3065=CARTESIAN_POINT('',(-5.025,-20.3,6.9));
#3066=CARTESIAN_POINT('Origin',(0.,-20.3,6.9));
#3067=CARTESIAN_POINT('',(-5.025,-20.3,9.));
#3068=CARTESIAN_POINT('',(-5.025,-20.3,6.9));
#3069=CARTESIAN_POINT('Origin',(0.,-20.3,9.));
#3070=CARTESIAN_POINT('Origin',(0.,-20.3,6.9));
#3071=CARTESIAN_POINT('Origin',(-3.98983552758699,-26.8,0.2));
#3072=CARTESIAN_POINT('',(6.25103652921323,-26.6,0.));
#3073=CARTESIAN_POINT('',(6.25103652921323,-26.6,0.));
#3074=CARTESIAN_POINT('',(-6.25103652921324,-26.6,0.));
#3075=CARTESIAN_POINT('',(-6.25103652921324,-27.,0.4));
#3076=CARTESIAN_POINT('',(-3.98983552758699,-26.6,0.));
#3077=CARTESIAN_POINT('Origin',(6.25103652921323,-25.,0.2));
#3078=CARTESIAN_POINT('',(7.8242989887542,-25.2912820512821,0.));
#3079=CARTESIAN_POINT('',(8.21761460363944,-25.3641025641026,0.4));
#3080=CARTESIAN_POINT('',(7.8242989887542,-25.2912820512821,0.));
#3081=CARTESIAN_POINT('Origin',(6.25103652921323,-25.,0.4));
#3082=CARTESIAN_POINT('Origin',(6.25103652921323,-25.,0.));
#3083=CARTESIAN_POINT('Origin',(29.26,-29.26,0.2));
#3084=CARTESIAN_POINT('',(25.2912820512821,-7.82429898875421,0.));
#3085=CARTESIAN_POINT('Origin',(29.26,-29.26,0.));
#3086=CARTESIAN_POINT('',(25.3641025641026,-8.21761460363945,0.4));
#3087=CARTESIAN_POINT('',(25.2912820512821,-7.82429898875421,0.));
#3088=CARTESIAN_POINT('Origin',(29.26,-29.26,0.4));
#3089=CARTESIAN_POINT('Origin',(25.,-6.25103652921323,0.2));
#3090=CARTESIAN_POINT('',(26.6,-6.25103652921323,0.));
#3091=CARTESIAN_POINT('',(26.6,-6.25103652921323,0.));
#3092=CARTESIAN_POINT('Origin',(25.,-6.25103652921323,0.4));
#3093=CARTESIAN_POINT('Origin',(25.,-6.25103652921323,0.));
#3094=CARTESIAN_POINT('Origin',(26.8,-3.98983552758699,0.2));
#3095=CARTESIAN_POINT('',(26.6,6.25103652921323,0.));
#3096=CARTESIAN_POINT('',(26.6,6.25103652921323,0.));
#3097=CARTESIAN_POINT('',(26.6,-3.98983552758699,0.));
#3098=CARTESIAN_POINT('Origin',(25.,6.25103652921323,0.2));
#3099=CARTESIAN_POINT('',(25.2912820512821,7.82429898875421,0.));
#3100=CARTESIAN_POINT('',(25.3641025641026,8.21761460363946,0.4));
#3101=CARTESIAN_POINT('',(25.2912820512821,7.82429898875421,0.));
#3102=CARTESIAN_POINT('Origin',(25.,6.25103652921323,0.4));
#3103=CARTESIAN_POINT('Origin',(25.,6.25103652921323,0.));
#3104=CARTESIAN_POINT('Origin',(29.26,29.26,0.2));
#3105=CARTESIAN_POINT('',(7.82429898875421,25.2912820512821,0.));
#3106=CARTESIAN_POINT('Origin',(29.26,29.26,0.));
#3107=CARTESIAN_POINT('',(8.21761460363946,25.3641025641026,0.4));
#3108=CARTESIAN_POINT('',(7.82429898875421,25.2912820512821,0.));
#3109=CARTESIAN_POINT('Origin',(29.26,29.26,0.4));
#3110=CARTESIAN_POINT('Origin',(6.25103652921323,25.,0.2));
#3111=CARTESIAN_POINT('',(6.25103652921323,26.6,0.));
#3112=CARTESIAN_POINT('',(6.25103652921323,26.6,0.));
#3113=CARTESIAN_POINT('Origin',(6.25103652921323,25.,0.4));
#3114=CARTESIAN_POINT('Origin',(6.25103652921323,25.,0.));
#3115=CARTESIAN_POINT('Origin',(3.98983552758699,26.8,0.2));
#3116=CARTESIAN_POINT('',(-6.25103652921323,26.6,0.));
#3117=CARTESIAN_POINT('',(-6.25103652921323,26.6,0.));
#3118=CARTESIAN_POINT('',(3.98983552758699,26.6,0.));
#3119=CARTESIAN_POINT('Origin',(-6.25103652921323,25.,0.2));
#3120=CARTESIAN_POINT('',(-7.8242989887542,25.2912820512821,0.));
#3121=CARTESIAN_POINT('',(-8.21761460363945,25.3641025641026,0.4));
#3122=CARTESIAN_POINT('',(-7.8242989887542,25.2912820512821,0.));
#3123=CARTESIAN_POINT('Origin',(-6.25103652921323,25.,0.4));
#3124=CARTESIAN_POINT('Origin',(-6.25103652921323,25.,0.));
#3125=CARTESIAN_POINT('Origin',(-29.26,29.26,0.2));
#3126=CARTESIAN_POINT('',(-25.2912820512821,7.82429898875421,0.));
#3127=CARTESIAN_POINT('Origin',(-29.26,29.26,0.));
#3128=CARTESIAN_POINT('',(-25.3641025641026,8.21761460363946,0.4));
#3129=CARTESIAN_POINT('',(-25.2912820512821,7.82429898875421,0.));
#3130=CARTESIAN_POINT('Origin',(-29.26,29.26,0.4));
#3131=CARTESIAN_POINT('Origin',(-25.,6.25103652921323,0.2));
#3132=CARTESIAN_POINT('',(-26.6,6.25103652921323,0.));
#3133=CARTESIAN_POINT('',(-26.6,6.25103652921323,0.));
#3134=CARTESIAN_POINT('Origin',(-25.,6.25103652921323,0.4));
#3135=CARTESIAN_POINT('Origin',(-25.,6.25103652921323,0.));
#3136=CARTESIAN_POINT('Origin',(-26.8,3.98983552758699,0.2));
#3137=CARTESIAN_POINT('',(-26.6,-6.25103652921323,0.));
#3138=CARTESIAN_POINT('',(-26.6,-6.25103652921323,0.));
#3139=CARTESIAN_POINT('',(-26.6,3.98983552758699,0.));
#3140=CARTESIAN_POINT('Origin',(-25.,-6.25103652921323,0.2));
#3141=CARTESIAN_POINT('',(-25.2912820512821,-7.82429898875421,0.));
#3142=CARTESIAN_POINT('',(-25.3641025641026,-8.21761460363945,0.4));
#3143=CARTESIAN_POINT('',(-25.2912820512821,-7.82429898875421,0.));
#3144=CARTESIAN_POINT('Origin',(-25.,-6.25103652921323,0.4));
#3145=CARTESIAN_POINT('Origin',(-25.,-6.25103652921323,0.));
#3146=CARTESIAN_POINT('Origin',(-29.26,-29.26,0.2));
#3147=CARTESIAN_POINT('',(-7.82429898875422,-25.2912820512821,0.));
#3148=CARTESIAN_POINT('Origin',(-29.26,-29.26,0.));
#3149=CARTESIAN_POINT('',(-8.21761460363946,-25.3641025641026,0.4));
#3150=CARTESIAN_POINT('',(-7.82429898875422,-25.2912820512821,0.));
#3151=CARTESIAN_POINT('Origin',(-29.26,-29.26,0.4));
#3152=CARTESIAN_POINT('Origin',(-6.25103652921324,-25.,0.2));
#3153=CARTESIAN_POINT('Origin',(-6.25103652921324,-25.,0.4));
#3154=CARTESIAN_POINT('Origin',(-6.25103652921324,-25.,0.));
#3155=CARTESIAN_POINT('Origin',(-6.25103652921323,25.,0.));
#3156=CARTESIAN_POINT('',(-8.21761460363945,25.3641025641026,8.2));
#3157=CARTESIAN_POINT('',(-8.21761460363945,25.3641025641026,0.));
#3158=CARTESIAN_POINT('Origin',(-6.25103652921323,25.,8.2));
#3159=CARTESIAN_POINT('Origin',(-29.26,29.26,0.));
#3160=CARTESIAN_POINT('',(-25.3641025641026,8.21761460363946,8.2));
#3161=CARTESIAN_POINT('',(-25.3641025641026,8.21761460363946,0.));
#3162=CARTESIAN_POINT('Origin',(-29.26,29.26,8.2));
#3163=CARTESIAN_POINT('Origin',(-25.,6.25103652921323,0.));
#3164=CARTESIAN_POINT('Origin',(-25.,6.25103652921323,8.2));
#3165=CARTESIAN_POINT('Origin',(-25.,-6.25103652921323,0.));
#3166=CARTESIAN_POINT('',(-25.3641025641026,-8.21761460363945,8.2));
#3167=CARTESIAN_POINT('',(-25.3641025641026,-8.21761460363945,0.));
#3168=CARTESIAN_POINT('Origin',(-25.,-6.25103652921323,8.2));
#3169=CARTESIAN_POINT('Origin',(-29.26,-29.26,0.));
#3170=CARTESIAN_POINT('',(-8.21761460363946,-25.3641025641026,8.2));
#3171=CARTESIAN_POINT('',(-8.21761460363946,-25.3641025641026,0.));
#3172=CARTESIAN_POINT('Origin',(-29.26,-29.26,8.2));
#3173=CARTESIAN_POINT('Origin',(-6.25103652921324,-25.,0.));
#3174=CARTESIAN_POINT('Origin',(-6.25103652921324,-25.,8.2));
#3175=CARTESIAN_POINT('Origin',(0.,0.,0.));
#3176=CARTESIAN_POINT('',(-13.9,1.70225905081482E-15,0.));
#3177=CARTESIAN_POINT('Origin',(0.,0.,0.));
#3178=CARTESIAN_POINT('Origin',(0.,0.,0.2));
#3179=CARTESIAN_POINT('',(-13.5,-1.65327317884893E-15,0.4));
#3180=CARTESIAN_POINT('Origin',(0.,0.,0.4));
#3181=CARTESIAN_POINT('',(-13.7,-1.67776611483187E-15,0.2));
#3182=CARTESIAN_POINT('Origin',(0.,0.,0.));
#3183=CARTESIAN_POINT('',(-13.5,1.65327317884893E-15,8.2));
#3184=CARTESIAN_POINT('Origin',(0.,0.,8.2));
#3185=CARTESIAN_POINT('',(-13.5,-1.65327317884893E-15,0.));
#3186=CARTESIAN_POINT('Origin',(0.,0.,8.6));
#3187=CARTESIAN_POINT('',(-14.3,-1.75124492278072E-15,9.));
#3188=CARTESIAN_POINT('Origin',(0.,0.,9.));
#3189=CARTESIAN_POINT('',(-13.9,-1.70225905081482E-15,8.6));
#3190=CARTESIAN_POINT('Origin',(0.,0.,9.));
#3191=CARTESIAN_POINT('',(-7.43098337386896,25.2184615384615,9.));
#3192=CARTESIAN_POINT('',(-6.25103652921323,26.2,9.));
#3193=CARTESIAN_POINT('Origin',(-6.25103652921323,25.,9.));
#3194=CARTESIAN_POINT('',(-25.2184615384615,7.43098337386897,9.));
#3195=CARTESIAN_POINT('Origin',(-29.26,29.26,9.));
#3196=CARTESIAN_POINT('',(-26.2,6.25103652921323,9.));
#3197=CARTESIAN_POINT('Origin',(-25.,6.25103652921323,9.));
#3198=CARTESIAN_POINT('',(-26.2,-6.25103652921323,9.));
#3199=CARTESIAN_POINT('',(-26.2,3.98983552758699,9.));
#3200=CARTESIAN_POINT('',(-25.2184615384615,-7.43098337386896,9.));
#3201=CARTESIAN_POINT('Origin',(-25.,-6.25103652921323,9.));
#3202=CARTESIAN_POINT('',(-7.43098337386897,-25.2184615384615,9.));
#3203=CARTESIAN_POINT('Origin',(-29.26,-29.26,9.));
#3204=CARTESIAN_POINT('',(-6.25103652921324,-26.2,9.));
#3205=CARTESIAN_POINT('Origin',(-6.25103652921324,-25.,9.));
#3206=CARTESIAN_POINT('',(6.25103652921323,-26.2,9.));
#3207=CARTESIAN_POINT('',(-3.98983552758699,-26.2,9.));
#3208=CARTESIAN_POINT('',(7.43098337386896,-25.2184615384615,9.));
#3209=CARTESIAN_POINT('Origin',(6.25103652921323,-25.,9.));
#3210=CARTESIAN_POINT('',(25.2184615384615,-7.43098337386896,9.));
#3211=CARTESIAN_POINT('Origin',(29.26,-29.26,9.));
#3212=CARTESIAN_POINT('',(26.2,-6.25103652921323,9.));
#3213=CARTESIAN_POINT('Origin',(25.,-6.25103652921323,9.));
#3214=CARTESIAN_POINT('',(26.2,6.25103652921323,9.));
#3215=CARTESIAN_POINT('',(26.2,-3.98983552758699,9.));
#3216=CARTESIAN_POINT('',(25.2184615384615,7.43098337386897,9.));
#3217=CARTESIAN_POINT('Origin',(25.,6.25103652921323,9.));
#3218=CARTESIAN_POINT('',(7.43098337386897,25.2184615384615,9.));
#3219=CARTESIAN_POINT('Origin',(29.26,29.26,9.));
#3220=CARTESIAN_POINT('',(6.25103652921323,26.2,9.));
#3221=CARTESIAN_POINT('Origin',(6.25103652921323,25.,9.));
#3222=CARTESIAN_POINT('',(3.98983552758699,26.2,9.));
#3223=CARTESIAN_POINT('Origin',(-6.25103652921323,25.,8.6));
#3224=CARTESIAN_POINT('',(-6.25103652921323,26.2,9.));
#3225=CARTESIAN_POINT('',(-8.21761460363945,25.3641025641026,8.2));
#3226=CARTESIAN_POINT('Origin',(3.98983552758699,26.6,8.6));
#3227=CARTESIAN_POINT('',(6.25103652921323,26.2,9.));
#3228=CARTESIAN_POINT('Origin',(6.25103652921323,25.,8.6));
#3229=CARTESIAN_POINT('',(8.21761460363946,25.3641025641026,8.2));
#3230=CARTESIAN_POINT('',(7.43098337386897,25.2184615384615,9.));
#3231=CARTESIAN_POINT('Origin',(6.25103652921323,25.,8.2));
#3232=CARTESIAN_POINT('Origin',(29.26,29.26,8.6));
#3233=CARTESIAN_POINT('',(25.3641025641026,8.21761460363946,8.2));
#3234=CARTESIAN_POINT('',(25.2184615384615,7.43098337386897,9.));
#3235=CARTESIAN_POINT('Origin',(29.26,29.26,8.2));
#3236=CARTESIAN_POINT('Origin',(25.,6.25103652921323,8.6));
#3237=CARTESIAN_POINT('',(26.2,6.25103652921323,9.));
#3238=CARTESIAN_POINT('Origin',(25.,6.25103652921323,8.2));
#3239=CARTESIAN_POINT('Origin',(26.6,-3.98983552758699,8.6));
#3240=CARTESIAN_POINT('',(26.2,-6.25103652921323,9.));
#3241=CARTESIAN_POINT('Origin',(25.,-6.25103652921323,8.6));
#3242=CARTESIAN_POINT('',(25.3641025641026,-8.21761460363945,8.2));
#3243=CARTESIAN_POINT('',(25.2184615384615,-7.43098337386896,9.));
#3244=CARTESIAN_POINT('Origin',(25.,-6.25103652921323,8.2));
#3245=CARTESIAN_POINT('Origin',(29.26,-29.26,8.6));
#3246=CARTESIAN_POINT('',(8.21761460363944,-25.3641025641026,8.2));
#3247=CARTESIAN_POINT('',(7.43098337386896,-25.2184615384615,9.));
#3248=CARTESIAN_POINT('Origin',(29.26,-29.26,8.2));
#3249=CARTESIAN_POINT('Origin',(6.25103652921323,-25.,8.6));
#3250=CARTESIAN_POINT('',(6.25103652921323,-26.2,9.));
#3251=CARTESIAN_POINT('Origin',(6.25103652921323,-25.,8.2));
#3252=CARTESIAN_POINT('Origin',(-3.98983552758699,-26.6,8.6));
#3253=CARTESIAN_POINT('',(-6.25103652921324,-26.2,9.));
#3254=CARTESIAN_POINT('Origin',(-6.25103652921324,-25.,8.6));
#3255=CARTESIAN_POINT('',(-7.43098337386897,-25.2184615384615,9.));
#3256=CARTESIAN_POINT('Origin',(-29.26,-29.26,8.6));
#3257=CARTESIAN_POINT('',(-25.2184615384615,-7.43098337386896,9.));
#3258=CARTESIAN_POINT('Origin',(-25.,-6.25103652921323,8.6));
#3259=CARTESIAN_POINT('',(-26.2,-6.25103652921323,9.));
#3260=CARTESIAN_POINT('Origin',(-26.6,3.98983552758699,8.6));
#3261=CARTESIAN_POINT('',(-26.2,6.25103652921323,9.));
#3262=CARTESIAN_POINT('Origin',(-25.,6.25103652921323,8.6));
#3263=CARTESIAN_POINT('',(-25.2184615384615,7.43098337386897,9.));
#3264=CARTESIAN_POINT('Origin',(-29.26,29.26,8.6));
#3265=CARTESIAN_POINT('Origin',(6.25103652921323,-25.,0.));
#3266=CARTESIAN_POINT('',(8.21761460363944,-25.3641025641026,0.));
#3267=CARTESIAN_POINT('Origin',(25.,-6.25103652921323,0.));
#3268=CARTESIAN_POINT('',(25.3641025641026,-8.21761460363945,0.));
#3269=CARTESIAN_POINT('Origin',(25.,6.25103652921323,0.));
#3270=CARTESIAN_POINT('',(25.3641025641026,8.21761460363946,0.));
#3271=CARTESIAN_POINT('Origin',(6.25103652921323,25.,0.));
#3272=CARTESIAN_POINT('',(8.21761460363946,25.3641025641026,0.));
#3273=CARTESIAN_POINT('Origin',(29.26,29.26,0.));
#3274=CARTESIAN_POINT('Origin',(29.26,-29.26,0.));
#3275=CARTESIAN_POINT('',(0.,0.,0.));
#3276=CARTESIAN_POINT('Origin',(0.,0.,0.1));
#3277=CARTESIAN_POINT('',(-5.,6.12323399573677E-16,0.2));
#3278=CARTESIAN_POINT('Origin',(0.,0.,0.2));
#3279=CARTESIAN_POINT('',(-4.8,-5.87830463590729E-16,0.));
#3280=CARTESIAN_POINT('',(-4.9,-6.00076931582203E-16,0.1));
#3281=CARTESIAN_POINT('Origin',(0.,0.,0.));
#3282=CARTESIAN_POINT('Origin',(0.,0.,0.));
#3283=CARTESIAN_POINT('',(-5.,-6.12323399573677E-16,1.8));
#3284=CARTESIAN_POINT('Origin',(0.,0.,1.8));
#3285=CARTESIAN_POINT('',(-5.,-6.12323399573677E-16,0.));
#3286=CARTESIAN_POINT('Origin',(0.,0.,0.));
#3287=CARTESIAN_POINT('Origin',(0.,0.,1.9));
#3288=CARTESIAN_POINT('',(-4.8,5.87830463590729E-16,2.));
#3289=CARTESIAN_POINT('Origin',(0.,0.,2.));
#3290=CARTESIAN_POINT('',(-4.9,-6.00076931582203E-16,1.9));
#3291=CARTESIAN_POINT('Origin',(0.,0.,2.));
#3292=CARTESIAN_POINT('',(0.,0.,0.));
#3293=CARTESIAN_POINT('Origin',(0.,0.,0.));
#3294=CARTESIAN_POINT('',(-1.53080849893419E-16,-1.87469972832732E-32,2.5));
#3295=CARTESIAN_POINT('',(-1.53080849893419E-16,-1.87469972832732E-32,-2.5));
#3296=CARTESIAN_POINT('Origin',(0.,0.,0.));
#3297=CARTESIAN_POINT('',(0.,0.,0.));
#3298=CARTESIAN_POINT('Origin',(0.,1.,0.));
#3299=CARTESIAN_POINT('',(-2.25514051876985E-16,-1.,-1.22464679914735E-16));
#3300=CARTESIAN_POINT('Origin',(0.,0.,0.));
#3301=CARTESIAN_POINT('Origin',(0.125,0.,0.));
#3302=CARTESIAN_POINT('',(0.25,-1.25,-1.53080849893419E-16));
#3303=CARTESIAN_POINT('Origin',(0.25,0.,0.));
#3304=CARTESIAN_POINT('',(0.125,-1.125,-1.37772764904077E-16));
#3305=CARTESIAN_POINT('Origin',(5.,0.,0.));
#3306=CARTESIAN_POINT('',(9.75,-1.25,-1.53080849893419E-16));
#3307=CARTESIAN_POINT('Origin',(9.75,0.,0.));
#3308=CARTESIAN_POINT('',(5.,-1.25,-1.53080849893419E-16));
#3309=CARTESIAN_POINT('Origin',(9.875,0.,0.));
#3310=CARTESIAN_POINT('',(10.,-1.,-1.22464679914735E-16));
#3311=CARTESIAN_POINT('Origin',(10.,0.,0.));
#3312=CARTESIAN_POINT('',(9.875,-1.125,-1.37772764904077E-16));
#3313=CARTESIAN_POINT('Origin',(10.,0.,0.));
#3314=CARTESIAN_POINT('',(0.,0.,0.));
#3315=CARTESIAN_POINT('',(0.,20.3,6.9));
#3316=CARTESIAN_POINT('',(0.,-20.3,6.9));
#3317=CARTESIAN_POINT('',(21.5,0.,8.47214438511238));
#3318=CARTESIAN_POINT('',(-21.5,0.,8.47214438511238));
#3319=CARTESIAN_POINT('',(17.,2.,5.3));
#3320=CARTESIAN_POINT('',(17.,-2.,5.3));
#3321=CARTESIAN_POINT('',(-2.,17.,5.3));
#3322=CARTESIAN_POINT('',(2.,17.,5.3));
#3323=CARTESIAN_POINT('',(-17.,-2.,5.3));
#3324=CARTESIAN_POINT('',(-17.,2.,5.3));
#3325=CARTESIAN_POINT('',(2.,-17.,5.3));
#3326=CARTESIAN_POINT('',(-2.,-17.,5.3));
#3327=UNCERTAINTY_MEASURE_WITH_UNIT(LENGTH_MEASURE(0.01),#3339,
'DISTANCE_ACCURACY_VALUE',
'Maximum model space distance between geometric entities at asserted c
onnectivities');
#3328=UNCERTAINTY_MEASURE_WITH_UNIT(LENGTH_MEASURE(0.01),#3339,
'DISTANCE_ACCURACY_VALUE',
'Maximum model space distance between geometric entities at asserted c
onnectivities');
#3329=UNCERTAINTY_MEASURE_WITH_UNIT(LENGTH_MEASURE(0.01),#3339,
'DISTANCE_ACCURACY_VALUE',
'Maximum model space distance between geometric entities at asserted c
onnectivities');
#3330=UNCERTAINTY_MEASURE_WITH_UNIT(LENGTH_MEASURE(0.01),#3339,
'DISTANCE_ACCURACY_VALUE',
'Maximum model space distance between geometric entities at asserted c
onnectivities');
#3331=UNCERTAINTY_MEASURE_WITH_UNIT(LENGTH_MEASURE(0.01),#3339,
'DISTANCE_ACCURACY_VALUE',
'Maximum model space distance between geometric entities at asserted c
onnectivities');
#3332=UNCERTAINTY_MEASURE_WITH_UNIT(LENGTH_MEASURE(0.01),#3339,
'DISTANCE_ACCURACY_VALUE',
'Maximum model space distance between geometric entities at asserted c
onnectivities');
#3333=(
GEOMETRIC_REPRESENTATION_CONTEXT(3)
GLOBAL_UNCERTAINTY_ASSIGNED_CONTEXT((#3327))
GLOBAL_UNIT_ASSIGNED_CONTEXT((#3339,#3341,#3342))
REPRESENTATION_CONTEXT('','3D')
);
#3334=(
GEOMETRIC_REPRESENTATION_CONTEXT(3)
GLOBAL_UNCERTAINTY_ASSIGNED_CONTEXT((#3328))
GLOBAL_UNIT_ASSIGNED_CONTEXT((#3339,#3341,#3342))
REPRESENTATION_CONTEXT('','3D')
);
#3335=(
GEOMETRIC_REPRESENTATION_CONTEXT(3)
GLOBAL_UNCERTAINTY_ASSIGNED_CONTEXT((#3329))
GLOBAL_UNIT_ASSIGNED_CONTEXT((#3339,#3341,#3342))
REPRESENTATION_CONTEXT('','3D')
);
#3336=(
GEOMETRIC_REPRESENTATION_CONTEXT(3)
GLOBAL_UNCERTAINTY_ASSIGNED_CONTEXT((#3330))
GLOBAL_UNIT_ASSIGNED_CONTEXT((#3339,#3341,#3342))
REPRESENTATION_CONTEXT('','3D')
);
#3337=(
GEOMETRIC_REPRESENTATION_CONTEXT(3)
GLOBAL_UNCERTAINTY_ASSIGNED_CONTEXT((#3331))
GLOBAL_UNIT_ASSIGNED_CONTEXT((#3339,#3341,#3342))
REPRESENTATION_CONTEXT('','3D')
);
#3338=(
GEOMETRIC_REPRESENTATION_CONTEXT(3)
GLOBAL_UNCERTAINTY_ASSIGNED_CONTEXT((#3332))
GLOBAL_UNIT_ASSIGNED_CONTEXT((#3339,#3341,#3342))
REPRESENTATION_CONTEXT('','3D')
);
#3339=(
LENGTH_UNIT()
NAMED_UNIT(*)
SI_UNIT(.MILLI.,.METRE.)
);
#3340=(
LENGTH_UNIT()
NAMED_UNIT(*)
SI_UNIT($,.METRE.)
);
#3341=(
NAMED_UNIT(*)
PLANE_ANGLE_UNIT()
SI_UNIT($,.RADIAN.)
);
#3342=(
NAMED_UNIT(*)
SI_UNIT($,.STERADIAN.)
SOLID_ANGLE_UNIT()
);
#3343=SHAPE_DEFINITION_REPRESENTATION(#3348,#3366);
#3344=SHAPE_DEFINITION_REPRESENTATION(#3349,#3367);
#3345=SHAPE_DEFINITION_REPRESENTATION(#3350,#3368);
#3346=SHAPE_DEFINITION_REPRESENTATION(#3351,#3369);
#3347=SHAPE_DEFINITION_REPRESENTATION(#3352,#3370);
#3348=PRODUCT_DEFINITION_SHAPE('',$,#3372);
#3349=PRODUCT_DEFINITION_SHAPE('',$,#3373);
#3350=PRODUCT_DEFINITION_SHAPE('',$,#3374);
#3351=PRODUCT_DEFINITION_SHAPE('',$,#3375);
#3352=PRODUCT_DEFINITION_SHAPE('',$,#3376);
#3353=PRODUCT_DEFINITION_SHAPE($,$,#50);
#3354=PRODUCT_DEFINITION_SHAPE($,$,#51);
#3355=PRODUCT_DEFINITION_SHAPE($,$,#52);
#3356=PRODUCT_DEFINITION_SHAPE($,$,#53);
#3357=PRODUCT_DEFINITION_SHAPE($,$,#54);
#3358=PRODUCT_DEFINITION_SHAPE($,$,#55);
#3359=PRODUCT_DEFINITION_SHAPE($,$,#56);
#3360=PRODUCT_DEFINITION_SHAPE($,$,#57);
#3361=PRODUCT_DEFINITION_SHAPE($,$,#58);
#3362=PRODUCT_DEFINITION_SHAPE($,$,#59);
#3363=PRODUCT_DEFINITION_SHAPE($,$,#60);
#3364=PRODUCT_DEFINITION_SHAPE($,$,#61);
#3365=PRODUCT_DEFINITION_SHAPE($,$,#62);
#3366=SHAPE_REPRESENTATION('',(#1623,#1805,#1806,#1807,#1808,#1809,#1810,
#1811,#1812,#1813,#1814,#1815,#1816,#1817),#3333);
#3367=SHAPE_REPRESENTATION('',(#1624),#3334);
#3368=SHAPE_REPRESENTATION('',(#1782),#3335);
#3369=SHAPE_REPRESENTATION('',(#1792),#3336);
#3370=SHAPE_REPRESENTATION('',(#1795),#3337);
#3371=PRODUCT_DEFINITION_CONTEXT('part definition',#3388,'design');
#3372=PRODUCT_DEFINITION('2026-10-11-08-53-15-679','MAS-363',#3377,#3371);
#3373=PRODUCT_DEFINITION('2026-10-11-08-53-15-906',
'01_Coupler_Body_CNC_6061',#3378,#3371);
#3374=PRODUCT_DEFINITION('2026-10-11-08-53-16-563',
'02_Neodymium_Disc_Magnet_N35_10x2',#3379,#3371);
#3375=PRODUCT_DEFINITION('2026-10-11-08-53-16-659',
'03_Steel_Ball_5mm_G10',#3380,#3371);
#3376=PRODUCT_DEFINITION('2026-10-11-08-53-16-748',
'04_ISO_8734_Pin_2.5x10',#3381,#3371);
#3377=PRODUCT_DEFINITION_FORMATION('',$,#3390);
#3378=PRODUCT_DEFINITION_FORMATION('',$,#3391);
#3379=PRODUCT_DEFINITION_FORMATION('',$,#3392);
#3380=PRODUCT_DEFINITION_FORMATION('',$,#3393);
#3381=PRODUCT_DEFINITION_FORMATION('',$,#3394);
#3382=PRODUCT_RELATED_PRODUCT_CATEGORY('MAS-363','MAS-363',(#3390));
#3383=PRODUCT_RELATED_PRODUCT_CATEGORY('01_Coupler_Body_CNC_6061',
'01_Coupler_Body_CNC_6061',(#3391));
#3384=PRODUCT_RELATED_PRODUCT_CATEGORY(
'02_Neodymium_Disc_Magnet_N35_10x2','02_Neodymium_Disc_Magnet_N35_10x2',
(#3392));
#3385=PRODUCT_RELATED_PRODUCT_CATEGORY('03_Steel_Ball_5mm_G10',
'03_Steel_Ball_5mm_G10',(#3393));
#3386=PRODUCT_RELATED_PRODUCT_CATEGORY('04_ISO_8734_Pin_2.5x10',
'04_ISO_8734_Pin_2.5x10',(#3394));
#3387=APPLICATION_PROTOCOL_DEFINITION('international standard',
'automotive_design',2009,#3388);
#3388=APPLICATION_CONTEXT(
'Core Data for Automotive Mechanical Design Process');
#3389=PRODUCT_CONTEXT('part definition',#3388,'mechanical');
#3390=PRODUCT('2026-10-11-08-53-15-679','MAS-363',$,(#3389));
#3391=PRODUCT('2026-10-11-08-53-15-906','01_Coupler_Body_CNC_6061',$,(#3389));
#3392=PRODUCT('2026-10-11-08-53-16-563',
'02_Neodymium_Disc_Magnet_N35_10x2',$,(#3389));
#3393=PRODUCT('2026-10-11-08-53-16-659','03_Steel_Ball_5mm_G10',$,(#3389));
#3394=PRODUCT('2026-10-11-08-53-16-748','04_ISO_8734_Pin_2.5x10',$,(#3389));
#3395=PRESENTATION_STYLE_ASSIGNMENT((#3400));
#3396=PRESENTATION_STYLE_ASSIGNMENT((#3401));
#3397=PRESENTATION_STYLE_ASSIGNMENT((#3402));
#3398=PRESENTATION_STYLE_ASSIGNMENT((#3403));
#3399=PRESENTATION_STYLE_ASSIGNMENT((#3404));
#3400=SURFACE_STYLE_USAGE(.BOTH.,#3405);
#3401=SURFACE_STYLE_USAGE(.BOTH.,#3406);
#3402=SURFACE_STYLE_USAGE(.BOTH.,#3407);
#3403=SURFACE_STYLE_USAGE(.BOTH.,#3408);
#3404=SURFACE_STYLE_USAGE(.BOTH.,#3409);
#3405=SURFACE_SIDE_STYLE('',(#3410));
#3406=SURFACE_SIDE_STYLE('',(#3411));
#3407=SURFACE_SIDE_STYLE('',(#3412));
#3408=SURFACE_SIDE_STYLE('',(#3413));
#3409=SURFACE_SIDE_STYLE('',(#3414));
#3410=SURFACE_STYLE_FILL_AREA(#3415);
#3411=SURFACE_STYLE_FILL_AREA(#3416);
#3412=SURFACE_STYLE_FILL_AREA(#3417);
#3413=SURFACE_STYLE_FILL_AREA(#3418);
#3414=SURFACE_STYLE_FILL_AREA(#3419);
#3415=FILL_AREA_STYLE('Steel - Satin',(#3420));
#3416=FILL_AREA_STYLE('MAS363_body',(#3421));
#3417=FILL_AREA_STYLE('MAS363_mag',(#3422));
#3418=FILL_AREA_STYLE('MAS363_ball',(#3423));
#3419=FILL_AREA_STYLE('MAS363_pin',(#3424));
#3420=FILL_AREA_STYLE_COLOUR('Steel - Satin',#3425);
#3421=FILL_AREA_STYLE_COLOUR('MAS363_body',#3426);
#3422=FILL_AREA_STYLE_COLOUR('MAS363_mag',#3427);
#3423=FILL_AREA_STYLE_COLOUR('MAS363_ball',#3428);
#3424=FILL_AREA_STYLE_COLOUR('MAS363_pin',#3429);
#3425=COLOUR_RGB('Steel - Satin',0.627450980392157,0.627450980392157,0.627450980392157);
#3426=COLOUR_RGB('MAS363_body',0.83921568627451,0.847058823529412,0.862745098039216);
#3427=COLOUR_RGB('MAS363_mag',0.768627450980392,0.745098039215686,0.698039215686274);
#3428=COLOUR_RGB('MAS363_ball',0.882352941176471,0.894117647058824,0.909803921568627);
#3429=COLOUR_RGB('MAS363_pin',0.807843137254902,0.815686274509804,0.831372549019608);
#3430=COLOUR_RGB('Dark Blue',0.08,0.2,0.34);
#3431=FILL_AREA_STYLE_COLOUR('',#3430);
#3432=FILL_AREA_STYLE('',(#3431));
#3433=SURFACE_STYLE_FILL_AREA(#3432);
#3434=SURFACE_SIDE_STYLE('',(#3433));
#3435=SURFACE_STYLE_USAGE(.BOTH.,#3434);
#3436=PRESENTATION_STYLE_ASSIGNMENT((#3435));
#3437=COLOUR_RGB('Light Blue',0.38,0.62,0.78);
#3438=FILL_AREA_STYLE_COLOUR('',#3437);
#3439=FILL_AREA_STYLE('',(#3438));
#3440=SURFACE_STYLE_FILL_AREA(#3439);
#3441=SURFACE_SIDE_STYLE('',(#3440));
#3442=SURFACE_STYLE_USAGE(.BOTH.,#3441);
#3443=PRESENTATION_STYLE_ASSIGNMENT((#3442));
#3444=COLOUR_RGB('Sky Blue',0.24,0.69,0.87);
#3445=FILL_AREA_STYLE_COLOUR('',#3444);
#3446=FILL_AREA_STYLE('',(#3445));
#3447=SURFACE_STYLE_FILL_AREA(#3446);
#3448=SURFACE_SIDE_STYLE('',(#3447));
#3449=SURFACE_STYLE_USAGE(.BOTH.,#3448);
#3450=PRESENTATION_STYLE_ASSIGNMENT((#3449));
#3451=COLOUR_RGB('Grey',0.48,0.52,0.57);
#3452=FILL_AREA_STYLE_COLOUR('',#3451);
#3453=FILL_AREA_STYLE('',(#3452));
#3454=SURFACE_STYLE_FILL_AREA(#3453);
#3455=SURFACE_SIDE_STYLE('',(#3454));
#3456=SURFACE_STYLE_USAGE(.BOTH.,#3455);
#3457=PRESENTATION_STYLE_ASSIGNMENT((#3456));
#3458=COLOUR_RGB('Black',0.12,0.14,0.17);
#3459=FILL_AREA_STYLE_COLOUR('',#3458);
#3460=FILL_AREA_STYLE('',(#3459));
#3461=SURFACE_STYLE_FILL_AREA(#3460);
#3462=SURFACE_SIDE_STYLE('',(#3461));
#3463=SURFACE_STYLE_USAGE(.BOTH.,#3462);
#3464=PRESENTATION_STYLE_ASSIGNMENT((#3463));
#3465=COLOUR_RGB('Off White',0.89,0.88,0.83);
#3466=FILL_AREA_STYLE_COLOUR('',#3465);
#3467=FILL_AREA_STYLE('',(#3466));
#3468=SURFACE_STYLE_FILL_AREA(#3467);
#3469=SURFACE_SIDE_STYLE('',(#3468));
#3470=SURFACE_STYLE_USAGE(.BOTH.,#3469);
#3471=PRESENTATION_STYLE_ASSIGNMENT((#3470));
ENDSEC;
END-ISO-10303-21;
